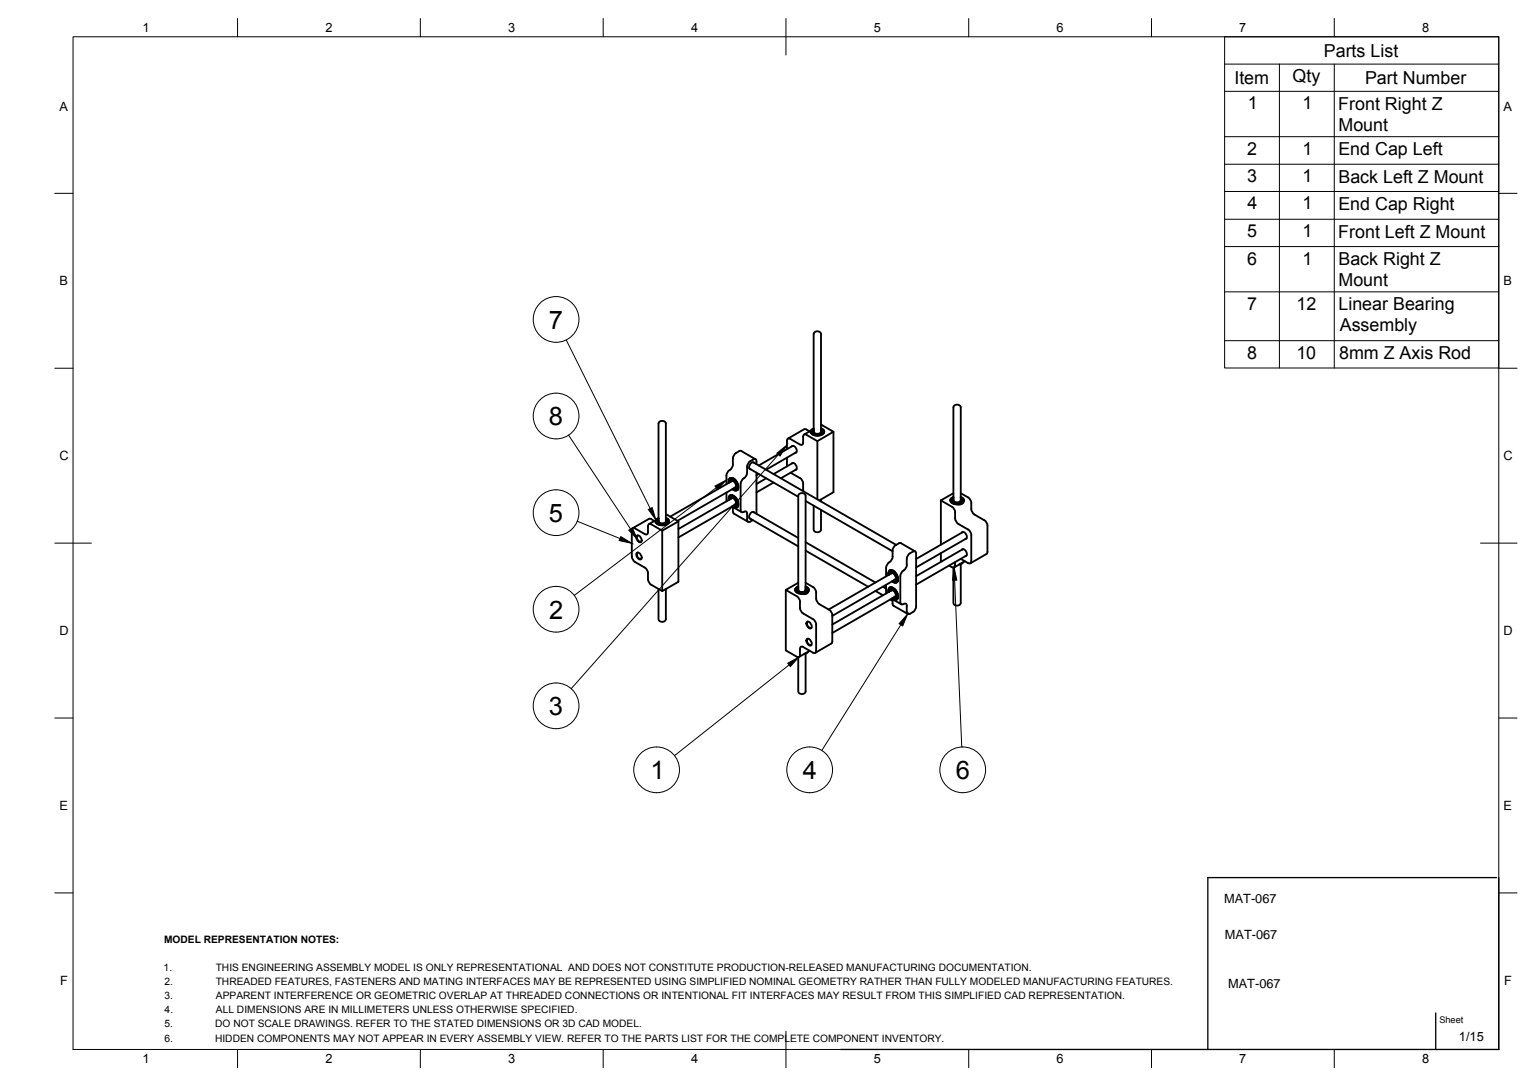
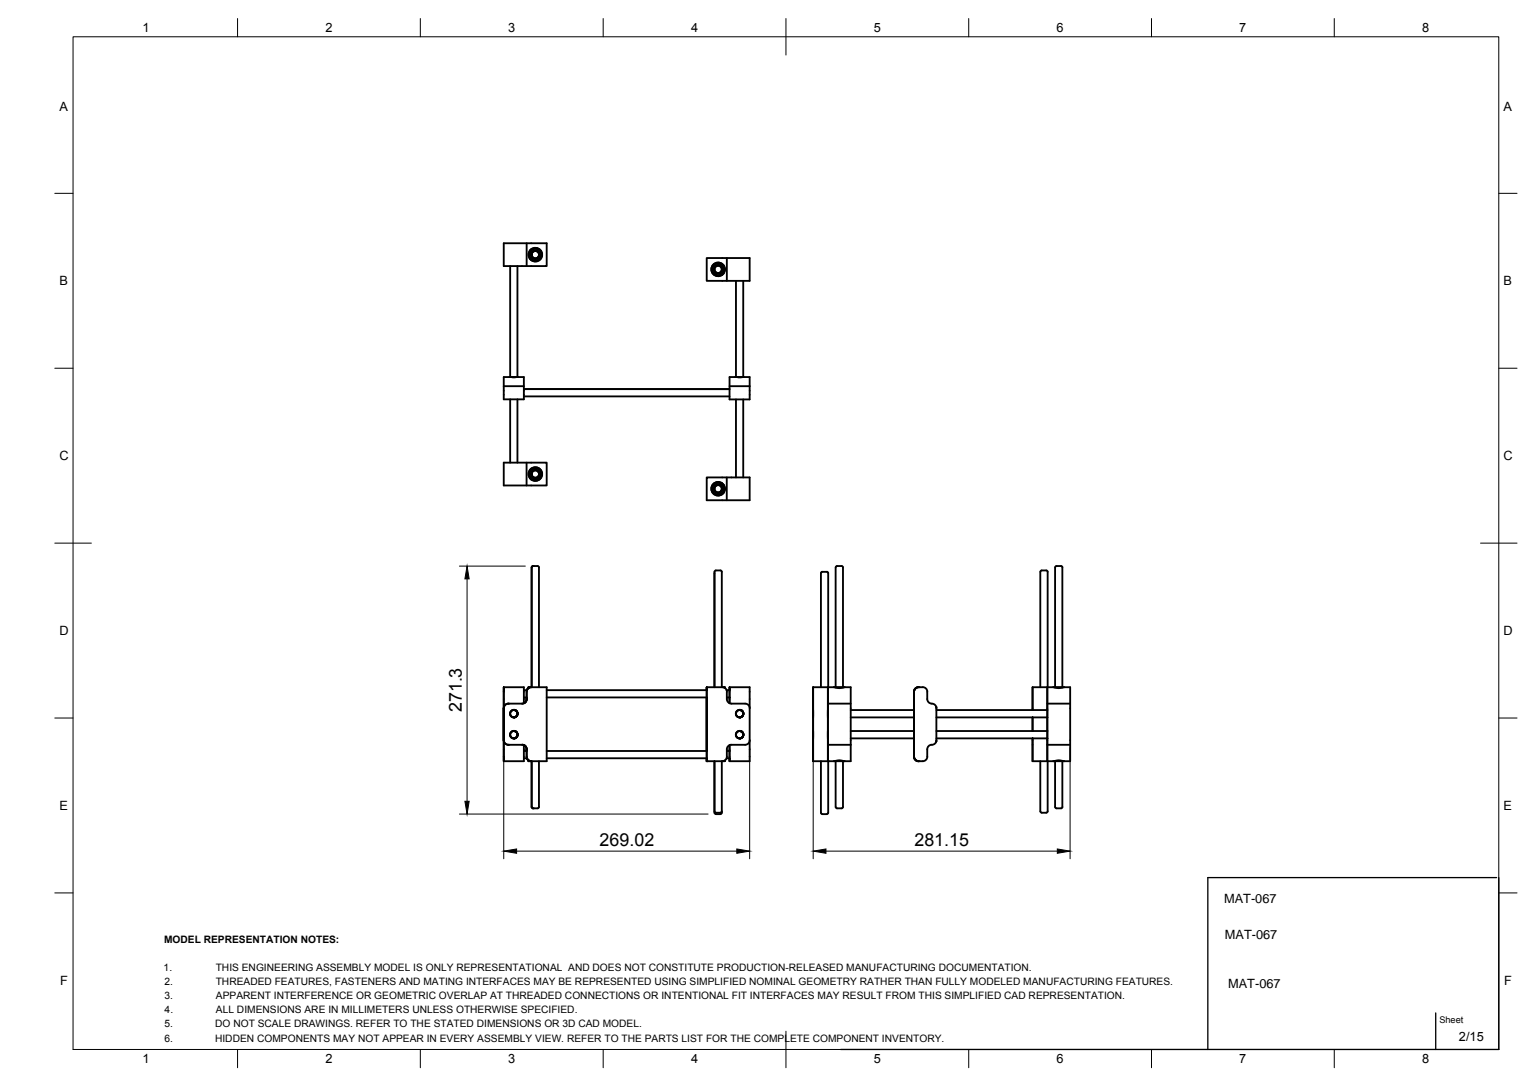
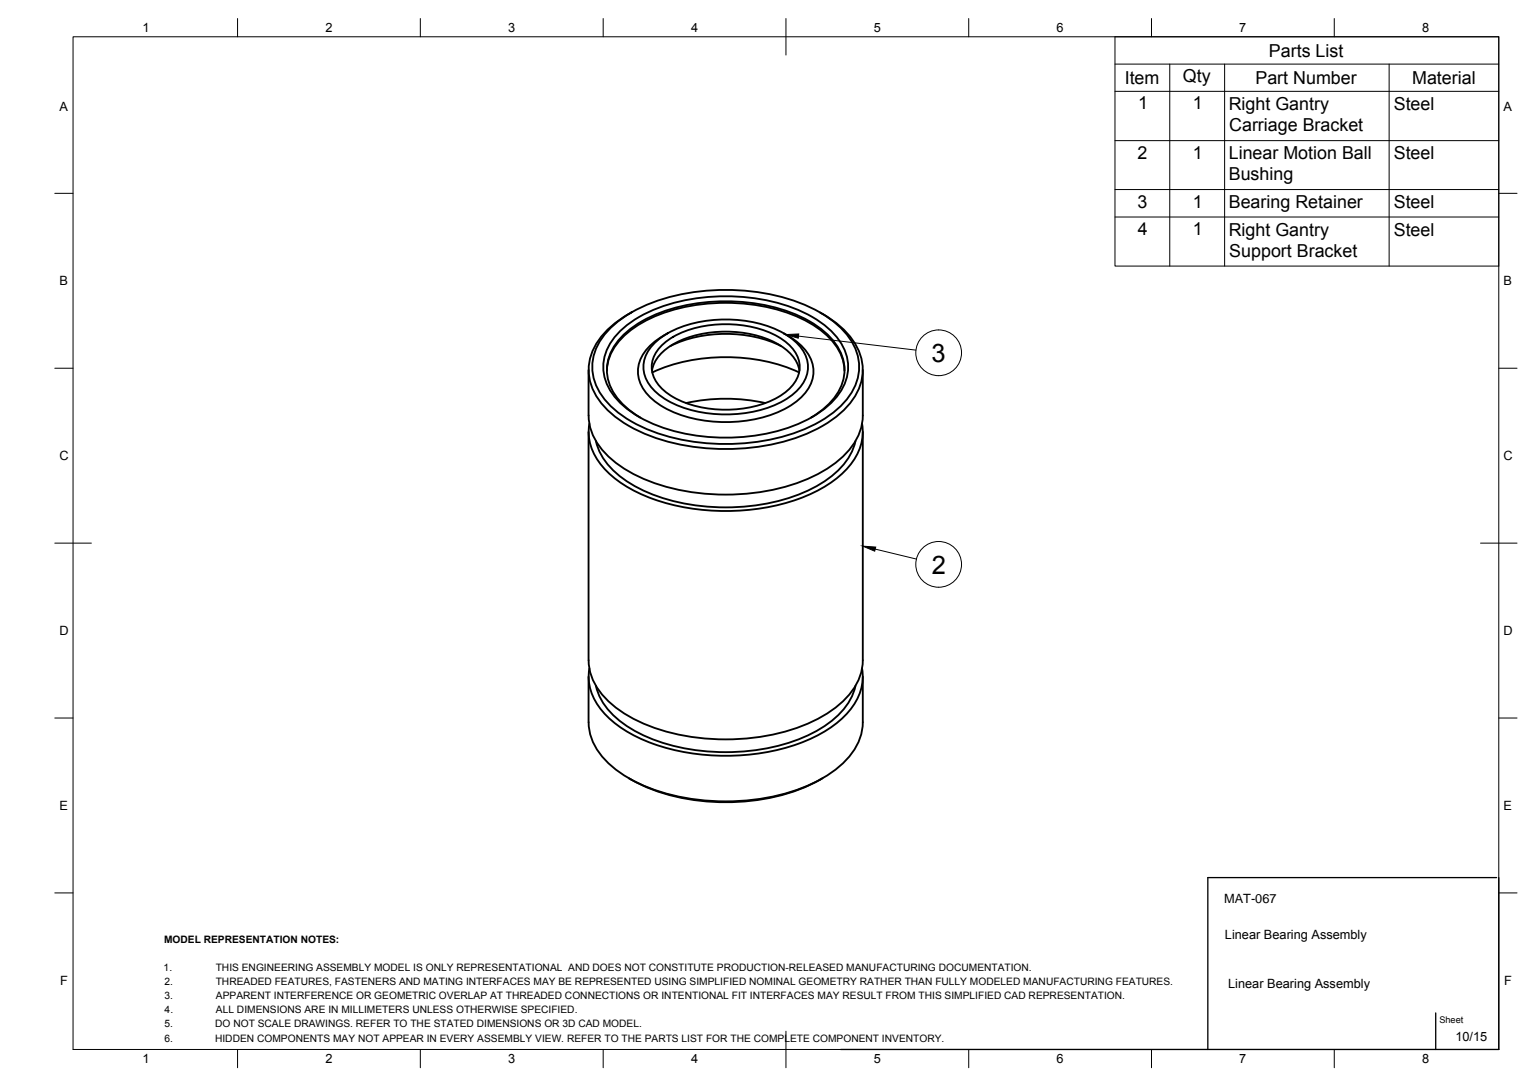
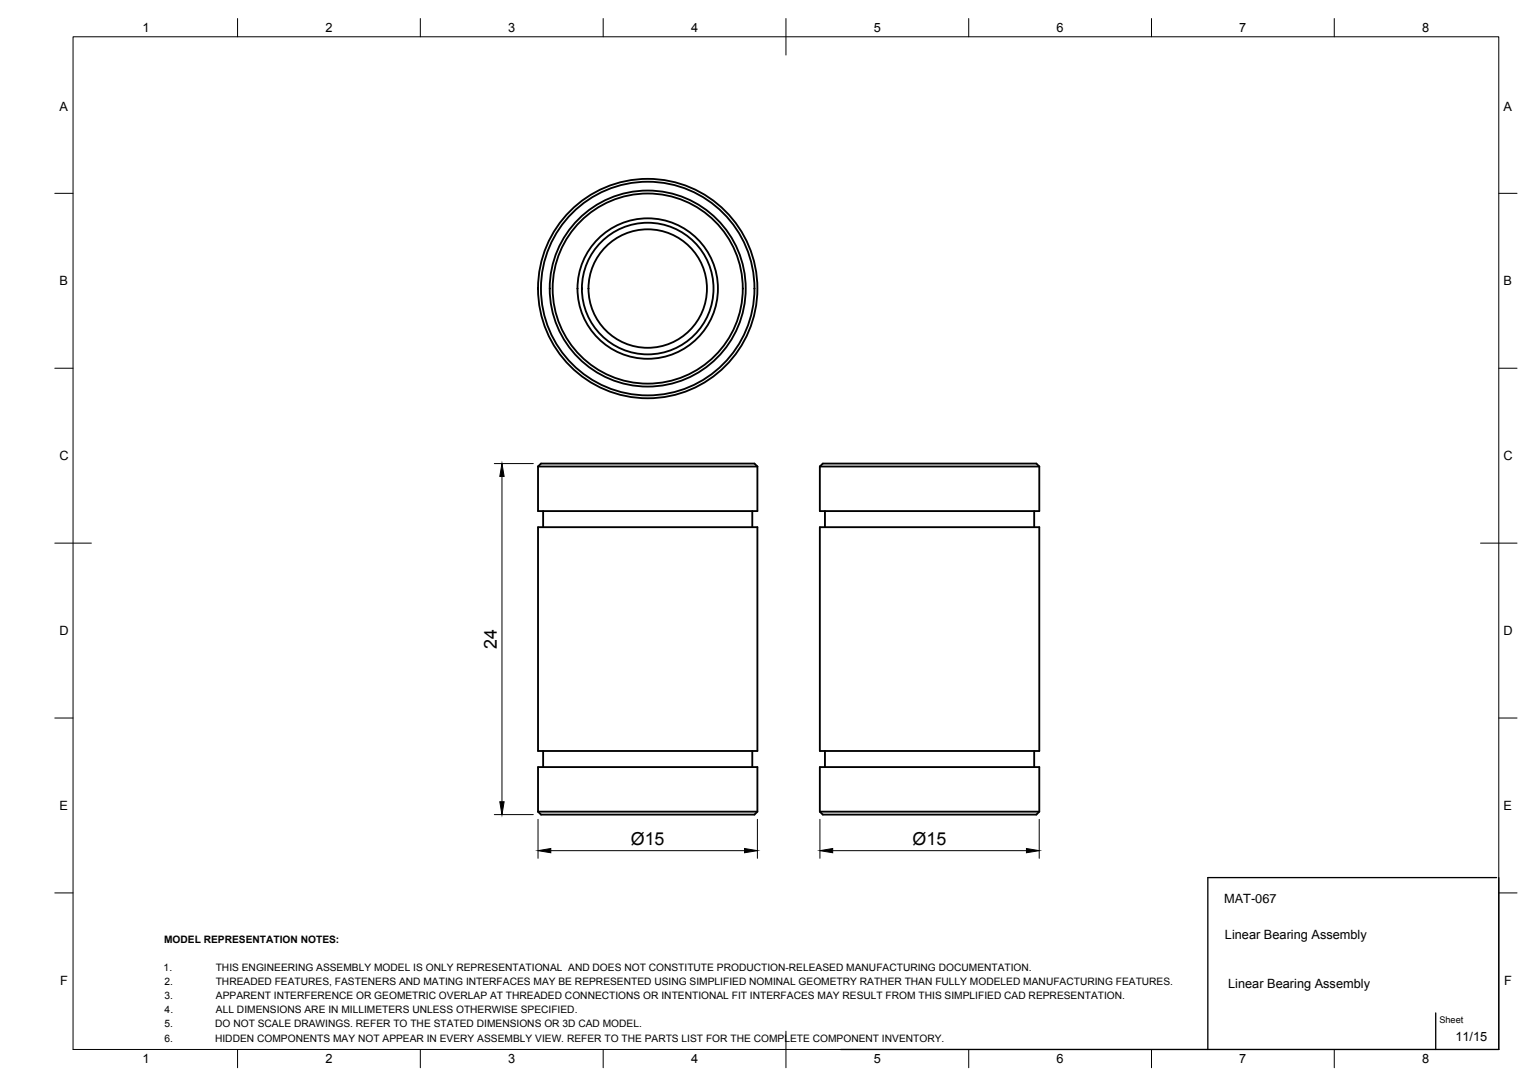
ISO-10303-21;
HEADER;
/* Generated by software containing ST-Developer
 * from STEP Tools, Inc. (www.steptools.com) 
 */

FILE_DESCRIPTION(
/* description */ ('CAx-IF Rec.Pracs.---Representation and Presentation of Product Manufa
cturing Information (PMI)---4.0---2014-10-13'),
/* implementation_level */ '2;1');

FILE_NAME(
/* name */ 'MAT-067',
/* time_stamp */ '2026-10-24T16:02:03-07:00',
/* author */ (''),
/* organization */ (''),
/* preprocessor_version */ 'ST-DEVELOPER v20.2',
/* originating_system */ 'Autodesk Translation Framework v15.17.0.0',
/* authorisation */ '');

FILE_SCHEMA (('AP242_MANAGED_MODEL_BASED_3D_ENGINEERING_MIM_LF { 1 0 10303 442 2 1 4 }'));
ENDSEC;

DATA;
#10=MECHANICAL_DESIGN_GEOMETRIC_PRESENTATION_REPRESENTATION('',(#349,#350,
#351,#352,#353,#354,#355,#356,#357,#358,#359),#6348);
#11=ITEM_DEFINED_TRANSFORMATION($,$,#3804,#3904);
#12=ITEM_DEFINED_TRANSFORMATION($,$,#3865,#3905);
#13=ITEM_DEFINED_TRANSFORMATION($,$,#3880,#3906);
#14=ITEM_DEFINED_TRANSFORMATION($,$,#3895,#3907);
#15=ITEM_DEFINED_TRANSFORMATION($,$,#3804,#3908);
#16=ITEM_DEFINED_TRANSFORMATION($,$,#3865,#3909);
#17=ITEM_DEFINED_TRANSFORMATION($,$,#3880,#3910);
#18=ITEM_DEFINED_TRANSFORMATION($,$,#3895,#3911);
#19=ITEM_DEFINED_TRANSFORMATION($,$,#3804,#3912);
#20=ITEM_DEFINED_TRANSFORMATION($,$,#3865,#3913);
#21=ITEM_DEFINED_TRANSFORMATION($,$,#3880,#3914);
#22=ITEM_DEFINED_TRANSFORMATION($,$,#3895,#3915);
#23=ITEM_DEFINED_TRANSFORMATION($,$,#3804,#3916);
#24=ITEM_DEFINED_TRANSFORMATION($,$,#3865,#3917);
#25=ITEM_DEFINED_TRANSFORMATION($,$,#3880,#3918);
#26=ITEM_DEFINED_TRANSFORMATION($,$,#3895,#3919);
#27=ITEM_DEFINED_TRANSFORMATION($,$,#3804,#3920);
#28=ITEM_DEFINED_TRANSFORMATION($,$,#3865,#3921);
#29=ITEM_DEFINED_TRANSFORMATION($,$,#3880,#3922);
#30=ITEM_DEFINED_TRANSFORMATION($,$,#3895,#3923);
#31=ITEM_DEFINED_TRANSFORMATION($,$,#3804,#3924);
#32=ITEM_DEFINED_TRANSFORMATION($,$,#3865,#3925);
#33=ITEM_DEFINED_TRANSFORMATION($,$,#3880,#3926);
#34=ITEM_DEFINED_TRANSFORMATION($,$,#3895,#3927);
#35=ITEM_DEFINED_TRANSFORMATION($,$,#3804,#3928);
#36=ITEM_DEFINED_TRANSFORMATION($,$,#3865,#3929);
#37=ITEM_DEFINED_TRANSFORMATION($,$,#3880,#3930);
#38=ITEM_DEFINED_TRANSFORMATION($,$,#3895,#3931);
#39=ITEM_DEFINED_TRANSFORMATION($,$,#3804,#3932);
#40=ITEM_DEFINED_TRANSFORMATION($,$,#3865,#3933);
#41=ITEM_DEFINED_TRANSFORMATION($,$,#3880,#3934);
#42=ITEM_DEFINED_TRANSFORMATION($,$,#3895,#3935);
#43=ITEM_DEFINED_TRANSFORMATION($,$,#3804,#3936);
#44=ITEM_DEFINED_TRANSFORMATION($,$,#3865,#3937);
#45=ITEM_DEFINED_TRANSFORMATION($,$,#3880,#3938);
#46=ITEM_DEFINED_TRANSFORMATION($,$,#3895,#3939);
#47=ITEM_DEFINED_TRANSFORMATION($,$,#3804,#3940);
#48=ITEM_DEFINED_TRANSFORMATION($,$,#3865,#3941);
#49=ITEM_DEFINED_TRANSFORMATION($,$,#3880,#3942);
#50=ITEM_DEFINED_TRANSFORMATION($,$,#3895,#3943);
#51=ITEM_DEFINED_TRANSFORMATION($,$,#3804,#3944);
#52=ITEM_DEFINED_TRANSFORMATION($,$,#3865,#3945);
#53=ITEM_DEFINED_TRANSFORMATION($,$,#3880,#3946);
#54=ITEM_DEFINED_TRANSFORMATION($,$,#3895,#3947);
#55=ITEM_DEFINED_TRANSFORMATION($,$,#3804,#3948);
#56=ITEM_DEFINED_TRANSFORMATION($,$,#3865,#3949);
#57=ITEM_DEFINED_TRANSFORMATION($,$,#3880,#3950);
#58=ITEM_DEFINED_TRANSFORMATION($,$,#3895,#3951);
#59=ITEM_DEFINED_TRANSFORMATION($,$,#3522,#3952);
#60=ITEM_DEFINED_TRANSFORMATION($,$,#3562,#3953);
#61=ITEM_DEFINED_TRANSFORMATION($,$,#3602,#3954);
#62=ITEM_DEFINED_TRANSFORMATION($,$,#3642,#3955);
#63=ITEM_DEFINED_TRANSFORMATION($,$,#3682,#3956);
#64=ITEM_DEFINED_TRANSFORMATION($,$,#3779,#3957);
#65=ITEM_DEFINED_TRANSFORMATION($,$,#3779,#3958);
#66=ITEM_DEFINED_TRANSFORMATION($,$,#3779,#3959);
#67=ITEM_DEFINED_TRANSFORMATION($,$,#3779,#3960);
#68=ITEM_DEFINED_TRANSFORMATION($,$,#3779,#3961);
#69=ITEM_DEFINED_TRANSFORMATION($,$,#3779,#3962);
#70=ITEM_DEFINED_TRANSFORMATION($,$,#3779,#3963);
#71=ITEM_DEFINED_TRANSFORMATION($,$,#3683,#3964);
#72=ITEM_DEFINED_TRANSFORMATION($,$,#3731,#3965);
#73=ITEM_DEFINED_TRANSFORMATION($,$,#3779,#3966);
#74=ITEM_DEFINED_TRANSFORMATION($,$,#3779,#3967);
#75=ITEM_DEFINED_TRANSFORMATION($,$,#3779,#3968);
#76=ITEM_DEFINED_TRANSFORMATION($,$,#3793,#3969);
#77=ITEM_DEFINED_TRANSFORMATION($,$,#3794,#3970);
#78=ITEM_DEFINED_TRANSFORMATION($,$,#3795,#3971);
#79=ITEM_DEFINED_TRANSFORMATION($,$,#3796,#3972);
#80=ITEM_DEFINED_TRANSFORMATION($,$,#3797,#3973);
#81=ITEM_DEFINED_TRANSFORMATION($,$,#3798,#3974);
#82=ITEM_DEFINED_TRANSFORMATION($,$,#3799,#3975);
#83=ITEM_DEFINED_TRANSFORMATION($,$,#3800,#3976);
#84=ITEM_DEFINED_TRANSFORMATION($,$,#3801,#3977);
#85=ITEM_DEFINED_TRANSFORMATION($,$,#3802,#3978);
#86=ITEM_DEFINED_TRANSFORMATION($,$,#3803,#3979);
#87=(
REPRESENTATION_RELATIONSHIP($,$,#6496,#6481)
REPRESENTATION_RELATIONSHIP_WITH_TRANSFORMATION(#11)
SHAPE_REPRESENTATION_RELATIONSHIP()
);
#88=(
REPRESENTATION_RELATIONSHIP($,$,#6497,#6481)
REPRESENTATION_RELATIONSHIP_WITH_TRANSFORMATION(#12)
SHAPE_REPRESENTATION_RELATIONSHIP()
);
#89=(
REPRESENTATION_RELATIONSHIP($,$,#6498,#6481)
REPRESENTATION_RELATIONSHIP_WITH_TRANSFORMATION(#13)
SHAPE_REPRESENTATION_RELATIONSHIP()
);
#90=(
REPRESENTATION_RELATIONSHIP($,$,#6499,#6481)
REPRESENTATION_RELATIONSHIP_WITH_TRANSFORMATION(#14)
SHAPE_REPRESENTATION_RELATIONSHIP()
);
#91=(
REPRESENTATION_RELATIONSHIP($,$,#6496,#6485)
REPRESENTATION_RELATIONSHIP_WITH_TRANSFORMATION(#15)
SHAPE_REPRESENTATION_RELATIONSHIP()
);
#92=(
REPRESENTATION_RELATIONSHIP($,$,#6497,#6485)
REPRESENTATION_RELATIONSHIP_WITH_TRANSFORMATION(#16)
SHAPE_REPRESENTATION_RELATIONSHIP()
);
#93=(
REPRESENTATION_RELATIONSHIP($,$,#6498,#6485)
REPRESENTATION_RELATIONSHIP_WITH_TRANSFORMATION(#17)
SHAPE_REPRESENTATION_RELATIONSHIP()
);
#94=(
REPRESENTATION_RELATIONSHIP($,$,#6499,#6485)
REPRESENTATION_RELATIONSHIP_WITH_TRANSFORMATION(#18)
SHAPE_REPRESENTATION_RELATIONSHIP()
);
#95=(
REPRESENTATION_RELATIONSHIP($,$,#6496,#6486)
REPRESENTATION_RELATIONSHIP_WITH_TRANSFORMATION(#19)
SHAPE_REPRESENTATION_RELATIONSHIP()
);
#96=(
REPRESENTATION_RELATIONSHIP($,$,#6497,#6486)
REPRESENTATION_RELATIONSHIP_WITH_TRANSFORMATION(#20)
SHAPE_REPRESENTATION_RELATIONSHIP()
);
#97=(
REPRESENTATION_RELATIONSHIP($,$,#6498,#6486)
REPRESENTATION_RELATIONSHIP_WITH_TRANSFORMATION(#21)
SHAPE_REPRESENTATION_RELATIONSHIP()
);
#98=(
REPRESENTATION_RELATIONSHIP($,$,#6499,#6486)
REPRESENTATION_RELATIONSHIP_WITH_TRANSFORMATION(#22)
SHAPE_REPRESENTATION_RELATIONSHIP()
);
#99=(
REPRESENTATION_RELATIONSHIP($,$,#6496,#6487)
REPRESENTATION_RELATIONSHIP_WITH_TRANSFORMATION(#23)
SHAPE_REPRESENTATION_RELATIONSHIP()
);
#100=(
REPRESENTATION_RELATIONSHIP($,$,#6497,#6487)
REPRESENTATION_RELATIONSHIP_WITH_TRANSFORMATION(#24)
SHAPE_REPRESENTATION_RELATIONSHIP()
);
#101=(
REPRESENTATION_RELATIONSHIP($,$,#6498,#6487)
REPRESENTATION_RELATIONSHIP_WITH_TRANSFORMATION(#25)
SHAPE_REPRESENTATION_RELATIONSHIP()
);
#102=(
REPRESENTATION_RELATIONSHIP($,$,#6499,#6487)
REPRESENTATION_RELATIONSHIP_WITH_TRANSFORMATION(#26)
SHAPE_REPRESENTATION_RELATIONSHIP()
);
#103=(
REPRESENTATION_RELATIONSHIP($,$,#6496,#6488)
REPRESENTATION_RELATIONSHIP_WITH_TRANSFORMATION(#27)
SHAPE_REPRESENTATION_RELATIONSHIP()
);
#104=(
REPRESENTATION_RELATIONSHIP($,$,#6497,#6488)
REPRESENTATION_RELATIONSHIP_WITH_TRANSFORMATION(#28)
SHAPE_REPRESENTATION_RELATIONSHIP()
);
#105=(
REPRESENTATION_RELATIONSHIP($,$,#6498,#6488)
REPRESENTATION_RELATIONSHIP_WITH_TRANSFORMATION(#29)
SHAPE_REPRESENTATION_RELATIONSHIP()
);
#106=(
REPRESENTATION_RELATIONSHIP($,$,#6499,#6488)
REPRESENTATION_RELATIONSHIP_WITH_TRANSFORMATION(#30)
SHAPE_REPRESENTATION_RELATIONSHIP()
);
#107=(
REPRESENTATION_RELATIONSHIP($,$,#6496,#6489)
REPRESENTATION_RELATIONSHIP_WITH_TRANSFORMATION(#31)
SHAPE_REPRESENTATION_RELATIONSHIP()
);
#108=(
REPRESENTATION_RELATIONSHIP($,$,#6497,#6489)
REPRESENTATION_RELATIONSHIP_WITH_TRANSFORMATION(#32)
SHAPE_REPRESENTATION_RELATIONSHIP()
);
#109=(
REPRESENTATION_RELATIONSHIP($,$,#6498,#6489)
REPRESENTATION_RELATIONSHIP_WITH_TRANSFORMATION(#33)
SHAPE_REPRESENTATION_RELATIONSHIP()
);
#110=(
REPRESENTATION_RELATIONSHIP($,$,#6499,#6489)
REPRESENTATION_RELATIONSHIP_WITH_TRANSFORMATION(#34)
SHAPE_REPRESENTATION_RELATIONSHIP()
);
#111=(
REPRESENTATION_RELATIONSHIP($,$,#6496,#6490)
REPRESENTATION_RELATIONSHIP_WITH_TRANSFORMATION(#35)
SHAPE_REPRESENTATION_RELATIONSHIP()
);
#112=(
REPRESENTATION_RELATIONSHIP($,$,#6497,#6490)
REPRESENTATION_RELATIONSHIP_WITH_TRANSFORMATION(#36)
SHAPE_REPRESENTATION_RELATIONSHIP()
);
#113=(
REPRESENTATION_RELATIONSHIP($,$,#6498,#6490)
REPRESENTATION_RELATIONSHIP_WITH_TRANSFORMATION(#37)
SHAPE_REPRESENTATION_RELATIONSHIP()
);
#114=(
REPRESENTATION_RELATIONSHIP($,$,#6499,#6490)
REPRESENTATION_RELATIONSHIP_WITH_TRANSFORMATION(#38)
SHAPE_REPRESENTATION_RELATIONSHIP()
);
#115=(
REPRESENTATION_RELATIONSHIP($,$,#6496,#6491)
REPRESENTATION_RELATIONSHIP_WITH_TRANSFORMATION(#39)
SHAPE_REPRESENTATION_RELATIONSHIP()
);
#116=(
REPRESENTATION_RELATIONSHIP($,$,#6497,#6491)
REPRESENTATION_RELATIONSHIP_WITH_TRANSFORMATION(#40)
SHAPE_REPRESENTATION_RELATIONSHIP()
);
#117=(
REPRESENTATION_RELATIONSHIP($,$,#6498,#6491)
REPRESENTATION_RELATIONSHIP_WITH_TRANSFORMATION(#41)
SHAPE_REPRESENTATION_RELATIONSHIP()
);
#118=(
REPRESENTATION_RELATIONSHIP($,$,#6499,#6491)
REPRESENTATION_RELATIONSHIP_WITH_TRANSFORMATION(#42)
SHAPE_REPRESENTATION_RELATIONSHIP()
);
#119=(
REPRESENTATION_RELATIONSHIP($,$,#6496,#6492)
REPRESENTATION_RELATIONSHIP_WITH_TRANSFORMATION(#43)
SHAPE_REPRESENTATION_RELATIONSHIP()
);
#120=(
REPRESENTATION_RELATIONSHIP($,$,#6497,#6492)
REPRESENTATION_RELATIONSHIP_WITH_TRANSFORMATION(#44)
SHAPE_REPRESENTATION_RELATIONSHIP()
);
#121=(
REPRESENTATION_RELATIONSHIP($,$,#6498,#6492)
REPRESENTATION_RELATIONSHIP_WITH_TRANSFORMATION(#45)
SHAPE_REPRESENTATION_RELATIONSHIP()
);
#122=(
REPRESENTATION_RELATIONSHIP($,$,#6499,#6492)
REPRESENTATION_RELATIONSHIP_WITH_TRANSFORMATION(#46)
SHAPE_REPRESENTATION_RELATIONSHIP()
);
#123=(
REPRESENTATION_RELATIONSHIP($,$,#6496,#6493)
REPRESENTATION_RELATIONSHIP_WITH_TRANSFORMATION(#47)
SHAPE_REPRESENTATION_RELATIONSHIP()
);
#124=(
REPRESENTATION_RELATIONSHIP($,$,#6497,#6493)
REPRESENTATION_RELATIONSHIP_WITH_TRANSFORMATION(#48)
SHAPE_REPRESENTATION_RELATIONSHIP()
);
#125=(
REPRESENTATION_RELATIONSHIP($,$,#6498,#6493)
REPRESENTATION_RELATIONSHIP_WITH_TRANSFORMATION(#49)
SHAPE_REPRESENTATION_RELATIONSHIP()
);
#126=(
REPRESENTATION_RELATIONSHIP($,$,#6499,#6493)
REPRESENTATION_RELATIONSHIP_WITH_TRANSFORMATION(#50)
SHAPE_REPRESENTATION_RELATIONSHIP()
);
#127=(
REPRESENTATION_RELATIONSHIP($,$,#6496,#6494)
REPRESENTATION_RELATIONSHIP_WITH_TRANSFORMATION(#51)
SHAPE_REPRESENTATION_RELATIONSHIP()
);
#128=(
REPRESENTATION_RELATIONSHIP($,$,#6497,#6494)
REPRESENTATION_RELATIONSHIP_WITH_TRANSFORMATION(#52)
SHAPE_REPRESENTATION_RELATIONSHIP()
);
#129=(
REPRESENTATION_RELATIONSHIP($,$,#6498,#6494)
REPRESENTATION_RELATIONSHIP_WITH_TRANSFORMATION(#53)
SHAPE_REPRESENTATION_RELATIONSHIP()
);
#130=(
REPRESENTATION_RELATIONSHIP($,$,#6499,#6494)
REPRESENTATION_RELATIONSHIP_WITH_TRANSFORMATION(#54)
SHAPE_REPRESENTATION_RELATIONSHIP()
);
#131=(
REPRESENTATION_RELATIONSHIP($,$,#6496,#6495)
REPRESENTATION_RELATIONSHIP_WITH_TRANSFORMATION(#55)
SHAPE_REPRESENTATION_RELATIONSHIP()
);
#132=(
REPRESENTATION_RELATIONSHIP($,$,#6497,#6495)
REPRESENTATION_RELATIONSHIP_WITH_TRANSFORMATION(#56)
SHAPE_REPRESENTATION_RELATIONSHIP()
);
#133=(
REPRESENTATION_RELATIONSHIP($,$,#6498,#6495)
REPRESENTATION_RELATIONSHIP_WITH_TRANSFORMATION(#57)
SHAPE_REPRESENTATION_RELATIONSHIP()
);
#134=(
REPRESENTATION_RELATIONSHIP($,$,#6499,#6495)
REPRESENTATION_RELATIONSHIP_WITH_TRANSFORMATION(#58)
SHAPE_REPRESENTATION_RELATIONSHIP()
);
#135=(
REPRESENTATION_RELATIONSHIP($,$,#6477,#6476)
REPRESENTATION_RELATIONSHIP_WITH_TRANSFORMATION(#59)
SHAPE_REPRESENTATION_RELATIONSHIP()
);
#136=(
REPRESENTATION_RELATIONSHIP($,$,#6478,#6476)
REPRESENTATION_RELATIONSHIP_WITH_TRANSFORMATION(#60)
SHAPE_REPRESENTATION_RELATIONSHIP()
);
#137=(
REPRESENTATION_RELATIONSHIP($,$,#6479,#6476)
REPRESENTATION_RELATIONSHIP_WITH_TRANSFORMATION(#61)
SHAPE_REPRESENTATION_RELATIONSHIP()
);
#138=(
REPRESENTATION_RELATIONSHIP($,$,#6480,#6476)
REPRESENTATION_RELATIONSHIP_WITH_TRANSFORMATION(#62)
SHAPE_REPRESENTATION_RELATIONSHIP()
);
#139=(
REPRESENTATION_RELATIONSHIP($,$,#6481,#6476)
REPRESENTATION_RELATIONSHIP_WITH_TRANSFORMATION(#63)
SHAPE_REPRESENTATION_RELATIONSHIP()
);
#140=(
REPRESENTATION_RELATIONSHIP($,$,#6484,#6476)
REPRESENTATION_RELATIONSHIP_WITH_TRANSFORMATION(#64)
SHAPE_REPRESENTATION_RELATIONSHIP()
);
#141=(
REPRESENTATION_RELATIONSHIP($,$,#6484,#6476)
REPRESENTATION_RELATIONSHIP_WITH_TRANSFORMATION(#65)
SHAPE_REPRESENTATION_RELATIONSHIP()
);
#142=(
REPRESENTATION_RELATIONSHIP($,$,#6484,#6476)
REPRESENTATION_RELATIONSHIP_WITH_TRANSFORMATION(#66)
SHAPE_REPRESENTATION_RELATIONSHIP()
);
#143=(
REPRESENTATION_RELATIONSHIP($,$,#6484,#6476)
REPRESENTATION_RELATIONSHIP_WITH_TRANSFORMATION(#67)
SHAPE_REPRESENTATION_RELATIONSHIP()
);
#144=(
REPRESENTATION_RELATIONSHIP($,$,#6484,#6476)
REPRESENTATION_RELATIONSHIP_WITH_TRANSFORMATION(#68)
SHAPE_REPRESENTATION_RELATIONSHIP()
);
#145=(
REPRESENTATION_RELATIONSHIP($,$,#6484,#6476)
REPRESENTATION_RELATIONSHIP_WITH_TRANSFORMATION(#69)
SHAPE_REPRESENTATION_RELATIONSHIP()
);
#146=(
REPRESENTATION_RELATIONSHIP($,$,#6484,#6476)
REPRESENTATION_RELATIONSHIP_WITH_TRANSFORMATION(#70)
SHAPE_REPRESENTATION_RELATIONSHIP()
);
#147=(
REPRESENTATION_RELATIONSHIP($,$,#6482,#6476)
REPRESENTATION_RELATIONSHIP_WITH_TRANSFORMATION(#71)
SHAPE_REPRESENTATION_RELATIONSHIP()
);
#148=(
REPRESENTATION_RELATIONSHIP($,$,#6483,#6476)
REPRESENTATION_RELATIONSHIP_WITH_TRANSFORMATION(#72)
SHAPE_REPRESENTATION_RELATIONSHIP()
);
#149=(
REPRESENTATION_RELATIONSHIP($,$,#6484,#6476)
REPRESENTATION_RELATIONSHIP_WITH_TRANSFORMATION(#73)
SHAPE_REPRESENTATION_RELATIONSHIP()
);
#150=(
REPRESENTATION_RELATIONSHIP($,$,#6484,#6476)
REPRESENTATION_RELATIONSHIP_WITH_TRANSFORMATION(#74)
SHAPE_REPRESENTATION_RELATIONSHIP()
);
#151=(
REPRESENTATION_RELATIONSHIP($,$,#6484,#6476)
REPRESENTATION_RELATIONSHIP_WITH_TRANSFORMATION(#75)
SHAPE_REPRESENTATION_RELATIONSHIP()
);
#152=(
REPRESENTATION_RELATIONSHIP($,$,#6485,#6476)
REPRESENTATION_RELATIONSHIP_WITH_TRANSFORMATION(#76)
SHAPE_REPRESENTATION_RELATIONSHIP()
);
#153=(
REPRESENTATION_RELATIONSHIP($,$,#6486,#6476)
REPRESENTATION_RELATIONSHIP_WITH_TRANSFORMATION(#77)
SHAPE_REPRESENTATION_RELATIONSHIP()
);
#154=(
REPRESENTATION_RELATIONSHIP($,$,#6487,#6476)
REPRESENTATION_RELATIONSHIP_WITH_TRANSFORMATION(#78)
SHAPE_REPRESENTATION_RELATIONSHIP()
);
#155=(
REPRESENTATION_RELATIONSHIP($,$,#6488,#6476)
REPRESENTATION_RELATIONSHIP_WITH_TRANSFORMATION(#79)
SHAPE_REPRESENTATION_RELATIONSHIP()
);
#156=(
REPRESENTATION_RELATIONSHIP($,$,#6489,#6476)
REPRESENTATION_RELATIONSHIP_WITH_TRANSFORMATION(#80)
SHAPE_REPRESENTATION_RELATIONSHIP()
);
#157=(
REPRESENTATION_RELATIONSHIP($,$,#6490,#6476)
REPRESENTATION_RELATIONSHIP_WITH_TRANSFORMATION(#81)
SHAPE_REPRESENTATION_RELATIONSHIP()
);
#158=(
REPRESENTATION_RELATIONSHIP($,$,#6491,#6476)
REPRESENTATION_RELATIONSHIP_WITH_TRANSFORMATION(#82)
SHAPE_REPRESENTATION_RELATIONSHIP()
);
#159=(
REPRESENTATION_RELATIONSHIP($,$,#6492,#6476)
REPRESENTATION_RELATIONSHIP_WITH_TRANSFORMATION(#83)
SHAPE_REPRESENTATION_RELATIONSHIP()
);
#160=(
REPRESENTATION_RELATIONSHIP($,$,#6493,#6476)
REPRESENTATION_RELATIONSHIP_WITH_TRANSFORMATION(#84)
SHAPE_REPRESENTATION_RELATIONSHIP()
);
#161=(
REPRESENTATION_RELATIONSHIP($,$,#6494,#6476)
REPRESENTATION_RELATIONSHIP_WITH_TRANSFORMATION(#85)
SHAPE_REPRESENTATION_RELATIONSHIP()
);
#162=(
REPRESENTATION_RELATIONSHIP($,$,#6495,#6476)
REPRESENTATION_RELATIONSHIP_WITH_TRANSFORMATION(#86)
SHAPE_REPRESENTATION_RELATIONSHIP()
);
#163=CONTEXT_DEPENDENT_SHAPE_REPRESENTATION(#87,#6400);
#164=CONTEXT_DEPENDENT_SHAPE_REPRESENTATION(#88,#6401);
#165=CONTEXT_DEPENDENT_SHAPE_REPRESENTATION(#89,#6402);
#166=CONTEXT_DEPENDENT_SHAPE_REPRESENTATION(#90,#6403);
#167=CONTEXT_DEPENDENT_SHAPE_REPRESENTATION(#91,#6404);
#168=CONTEXT_DEPENDENT_SHAPE_REPRESENTATION(#92,#6405);
#169=CONTEXT_DEPENDENT_SHAPE_REPRESENTATION(#93,#6406);
#170=CONTEXT_DEPENDENT_SHAPE_REPRESENTATION(#94,#6407);
#171=CONTEXT_DEPENDENT_SHAPE_REPRESENTATION(#95,#6408);
#172=CONTEXT_DEPENDENT_SHAPE_REPRESENTATION(#96,#6409);
#173=CONTEXT_DEPENDENT_SHAPE_REPRESENTATION(#97,#6410);
#174=CONTEXT_DEPENDENT_SHAPE_REPRESENTATION(#98,#6411);
#175=CONTEXT_DEPENDENT_SHAPE_REPRESENTATION(#99,#6412);
#176=CONTEXT_DEPENDENT_SHAPE_REPRESENTATION(#100,#6413);
#177=CONTEXT_DEPENDENT_SHAPE_REPRESENTATION(#101,#6414);
#178=CONTEXT_DEPENDENT_SHAPE_REPRESENTATION(#102,#6415);
#179=CONTEXT_DEPENDENT_SHAPE_REPRESENTATION(#103,#6416);
#180=CONTEXT_DEPENDENT_SHAPE_REPRESENTATION(#104,#6417);
#181=CONTEXT_DEPENDENT_SHAPE_REPRESENTATION(#105,#6418);
#182=CONTEXT_DEPENDENT_SHAPE_REPRESENTATION(#106,#6419);
#183=CONTEXT_DEPENDENT_SHAPE_REPRESENTATION(#107,#6420);
#184=CONTEXT_DEPENDENT_SHAPE_REPRESENTATION(#108,#6421);
#185=CONTEXT_DEPENDENT_SHAPE_REPRESENTATION(#109,#6422);
#186=CONTEXT_DEPENDENT_SHAPE_REPRESENTATION(#110,#6423);
#187=CONTEXT_DEPENDENT_SHAPE_REPRESENTATION(#111,#6424);
#188=CONTEXT_DEPENDENT_SHAPE_REPRESENTATION(#112,#6425);
#189=CONTEXT_DEPENDENT_SHAPE_REPRESENTATION(#113,#6426);
#190=CONTEXT_DEPENDENT_SHAPE_REPRESENTATION(#114,#6427);
#191=CONTEXT_DEPENDENT_SHAPE_REPRESENTATION(#115,#6428);
#192=CONTEXT_DEPENDENT_SHAPE_REPRESENTATION(#116,#6429);
#193=CONTEXT_DEPENDENT_SHAPE_REPRESENTATION(#117,#6430);
#194=CONTEXT_DEPENDENT_SHAPE_REPRESENTATION(#118,#6431);
#195=CONTEXT_DEPENDENT_SHAPE_REPRESENTATION(#119,#6432);
#196=CONTEXT_DEPENDENT_SHAPE_REPRESENTATION(#120,#6433);
#197=CONTEXT_DEPENDENT_SHAPE_REPRESENTATION(#121,#6434);
#198=CONTEXT_DEPENDENT_SHAPE_REPRESENTATION(#122,#6435);
#199=CONTEXT_DEPENDENT_SHAPE_REPRESENTATION(#123,#6436);
#200=CONTEXT_DEPENDENT_SHAPE_REPRESENTATION(#124,#6437);
#201=CONTEXT_DEPENDENT_SHAPE_REPRESENTATION(#125,#6438);
#202=CONTEXT_DEPENDENT_SHAPE_REPRESENTATION(#126,#6439);
#203=CONTEXT_DEPENDENT_SHAPE_REPRESENTATION(#127,#6440);
#204=CONTEXT_DEPENDENT_SHAPE_REPRESENTATION(#128,#6441);
#205=CONTEXT_DEPENDENT_SHAPE_REPRESENTATION(#129,#6442);
#206=CONTEXT_DEPENDENT_SHAPE_REPRESENTATION(#130,#6443);
#207=CONTEXT_DEPENDENT_SHAPE_REPRESENTATION(#131,#6444);
#208=CONTEXT_DEPENDENT_SHAPE_REPRESENTATION(#132,#6445);
#209=CONTEXT_DEPENDENT_SHAPE_REPRESENTATION(#133,#6446);
#210=CONTEXT_DEPENDENT_SHAPE_REPRESENTATION(#134,#6447);
#211=CONTEXT_DEPENDENT_SHAPE_REPRESENTATION(#135,#6448);
#212=CONTEXT_DEPENDENT_SHAPE_REPRESENTATION(#136,#6449);
#213=CONTEXT_DEPENDENT_SHAPE_REPRESENTATION(#137,#6450);
#214=CONTEXT_DEPENDENT_SHAPE_REPRESENTATION(#138,#6451);
#215=CONTEXT_DEPENDENT_SHAPE_REPRESENTATION(#139,#6452);
#216=CONTEXT_DEPENDENT_SHAPE_REPRESENTATION(#140,#6453);
#217=CONTEXT_DEPENDENT_SHAPE_REPRESENTATION(#141,#6454);
#218=CONTEXT_DEPENDENT_SHAPE_REPRESENTATION(#142,#6455);
#219=CONTEXT_DEPENDENT_SHAPE_REPRESENTATION(#143,#6456);
#220=CONTEXT_DEPENDENT_SHAPE_REPRESENTATION(#144,#6457);
#221=CONTEXT_DEPENDENT_SHAPE_REPRESENTATION(#145,#6458);
#222=CONTEXT_DEPENDENT_SHAPE_REPRESENTATION(#146,#6459);
#223=CONTEXT_DEPENDENT_SHAPE_REPRESENTATION(#147,#6460);
#224=CONTEXT_DEPENDENT_SHAPE_REPRESENTATION(#148,#6461);
#225=CONTEXT_DEPENDENT_SHAPE_REPRESENTATION(#149,#6462);
#226=CONTEXT_DEPENDENT_SHAPE_REPRESENTATION(#150,#6463);
#227=CONTEXT_DEPENDENT_SHAPE_REPRESENTATION(#151,#6464);
#228=CONTEXT_DEPENDENT_SHAPE_REPRESENTATION(#152,#6465);
#229=CONTEXT_DEPENDENT_SHAPE_REPRESENTATION(#153,#6466);
#230=CONTEXT_DEPENDENT_SHAPE_REPRESENTATION(#154,#6467);
#231=CONTEXT_DEPENDENT_SHAPE_REPRESENTATION(#155,#6468);
#232=CONTEXT_DEPENDENT_SHAPE_REPRESENTATION(#156,#6469);
#233=CONTEXT_DEPENDENT_SHAPE_REPRESENTATION(#157,#6470);
#234=CONTEXT_DEPENDENT_SHAPE_REPRESENTATION(#158,#6471);
#235=CONTEXT_DEPENDENT_SHAPE_REPRESENTATION(#159,#6472);
#236=CONTEXT_DEPENDENT_SHAPE_REPRESENTATION(#160,#6473);
#237=CONTEXT_DEPENDENT_SHAPE_REPRESENTATION(#161,#6474);
#238=CONTEXT_DEPENDENT_SHAPE_REPRESENTATION(#162,#6475);
#239=NEXT_ASSEMBLY_USAGE_OCCURRENCE('Linear Motion Ball Bushing:1',
'Linear Motion Ball Bushing:1','Linear Motion Ball Bushing:1',#6506,#6521,
'Linear Motion Ball Bushing:1');
#240=NEXT_ASSEMBLY_USAGE_OCCURRENCE('Right Gantry Carriage Bracket:1',
'Right Gantry Carriage Bracket:1','Right Gantry Carriage Bracket:1',#6506,
#6522,'Right Gantry Carriage Bracket:1');
#241=NEXT_ASSEMBLY_USAGE_OCCURRENCE('Bearing Retainer:1',
'Bearing Retainer:1','Bearing Retainer:1',#6506,#6523,
'Bearing Retainer:1');
#242=NEXT_ASSEMBLY_USAGE_OCCURRENCE('Right Gantry Support Bracket:1',
'Right Gantry Support Bracket:1','Right Gantry Support Bracket:1',#6506,
#6524,'Right Gantry Support Bracket:1');
#243=NEXT_ASSEMBLY_USAGE_OCCURRENCE('Linear Motion Ball Bushing:1',
'Linear Motion Ball Bushing:1','Linear Motion Ball Bushing:1',#6510,#6521,
'Linear Motion Ball Bushing:1');
#244=NEXT_ASSEMBLY_USAGE_OCCURRENCE('Right Gantry Carriage Bracket:1',
'Right Gantry Carriage Bracket:1','Right Gantry Carriage Bracket:1',#6510,
#6522,'Right Gantry Carriage Bracket:1');
#245=NEXT_ASSEMBLY_USAGE_OCCURRENCE('Bearing Retainer:1',
'Bearing Retainer:1','Bearing Retainer:1',#6510,#6523,
'Bearing Retainer:1');
#246=NEXT_ASSEMBLY_USAGE_OCCURRENCE('Right Gantry Support Bracket:1',
'Right Gantry Support Bracket:1','Right Gantry Support Bracket:1',#6510,
#6524,'Right Gantry Support Bracket:1');
#247=NEXT_ASSEMBLY_USAGE_OCCURRENCE('Linear Motion Ball Bushing:1',
'Linear Motion Ball Bushing:1','Linear Motion Ball Bushing:1',#6511,#6521,
'Linear Motion Ball Bushing:1');
#248=NEXT_ASSEMBLY_USAGE_OCCURRENCE('Right Gantry Carriage Bracket:1',
'Right Gantry Carriage Bracket:1','Right Gantry Carriage Bracket:1',#6511,
#6522,'Right Gantry Carriage Bracket:1');
#249=NEXT_ASSEMBLY_USAGE_OCCURRENCE('Bearing Retainer:1',
'Bearing Retainer:1','Bearing Retainer:1',#6511,#6523,
'Bearing Retainer:1');
#250=NEXT_ASSEMBLY_USAGE_OCCURRENCE('Right Gantry Support Bracket:1',
'Right Gantry Support Bracket:1','Right Gantry Support Bracket:1',#6511,
#6524,'Right Gantry Support Bracket:1');
#251=NEXT_ASSEMBLY_USAGE_OCCURRENCE('Linear Motion Ball Bushing:1',
'Linear Motion Ball Bushing:1','Linear Motion Ball Bushing:1',#6512,#6521,
'Linear Motion Ball Bushing:1');
#252=NEXT_ASSEMBLY_USAGE_OCCURRENCE('Right Gantry Carriage Bracket:1',
'Right Gantry Carriage Bracket:1','Right Gantry Carriage Bracket:1',#6512,
#6522,'Right Gantry Carriage Bracket:1');
#253=NEXT_ASSEMBLY_USAGE_OCCURRENCE('Bearing Retainer:1',
'Bearing Retainer:1','Bearing Retainer:1',#6512,#6523,
'Bearing Retainer:1');
#254=NEXT_ASSEMBLY_USAGE_OCCURRENCE('Right Gantry Support Bracket:1',
'Right Gantry Support Bracket:1','Right Gantry Support Bracket:1',#6512,
#6524,'Right Gantry Support Bracket:1');
#255=NEXT_ASSEMBLY_USAGE_OCCURRENCE('Linear Motion Ball Bushing:1',
'Linear Motion Ball Bushing:1','Linear Motion Ball Bushing:1',#6513,#6521,
'Linear Motion Ball Bushing:1');
#256=NEXT_ASSEMBLY_USAGE_OCCURRENCE('Right Gantry Carriage Bracket:1',
'Right Gantry Carriage Bracket:1','Right Gantry Carriage Bracket:1',#6513,
#6522,'Right Gantry Carriage Bracket:1');
#257=NEXT_ASSEMBLY_USAGE_OCCURRENCE('Bearing Retainer:1',
'Bearing Retainer:1','Bearing Retainer:1',#6513,#6523,
'Bearing Retainer:1');
#258=NEXT_ASSEMBLY_USAGE_OCCURRENCE('Right Gantry Support Bracket:1',
'Right Gantry Support Bracket:1','Right Gantry Support Bracket:1',#6513,
#6524,'Right Gantry Support Bracket:1');
#259=NEXT_ASSEMBLY_USAGE_OCCURRENCE('Linear Motion Ball Bushing:1',
'Linear Motion Ball Bushing:1','Linear Motion Ball Bushing:1',#6514,#6521,
'Linear Motion Ball Bushing:1');
#260=NEXT_ASSEMBLY_USAGE_OCCURRENCE('Right Gantry Carriage Bracket:1',
'Right Gantry Carriage Bracket:1','Right Gantry Carriage Bracket:1',#6514,
#6522,'Right Gantry Carriage Bracket:1');
#261=NEXT_ASSEMBLY_USAGE_OCCURRENCE('Bearing Retainer:1',
'Bearing Retainer:1','Bearing Retainer:1',#6514,#6523,
'Bearing Retainer:1');
#262=NEXT_ASSEMBLY_USAGE_OCCURRENCE('Right Gantry Support Bracket:1',
'Right Gantry Support Bracket:1','Right Gantry Support Bracket:1',#6514,
#6524,'Right Gantry Support Bracket:1');
#263=NEXT_ASSEMBLY_USAGE_OCCURRENCE('Linear Motion Ball Bushing:1',
'Linear Motion Ball Bushing:1','Linear Motion Ball Bushing:1',#6515,#6521,
'Linear Motion Ball Bushing:1');
#264=NEXT_ASSEMBLY_USAGE_OCCURRENCE('Right Gantry Carriage Bracket:1',
'Right Gantry Carriage Bracket:1','Right Gantry Carriage Bracket:1',#6515,
#6522,'Right Gantry Carriage Bracket:1');
#265=NEXT_ASSEMBLY_USAGE_OCCURRENCE('Bearing Retainer:1',
'Bearing Retainer:1','Bearing Retainer:1',#6515,#6523,
'Bearing Retainer:1');
#266=NEXT_ASSEMBLY_USAGE_OCCURRENCE('Right Gantry Support Bracket:1',
'Right Gantry Support Bracket:1','Right Gantry Support Bracket:1',#6515,
#6524,'Right Gantry Support Bracket:1');
#267=NEXT_ASSEMBLY_USAGE_OCCURRENCE('Linear Motion Ball Bushing:1',
'Linear Motion Ball Bushing:1','Linear Motion Ball Bushing:1',#6516,#6521,
'Linear Motion Ball Bushing:1');
#268=NEXT_ASSEMBLY_USAGE_OCCURRENCE('Right Gantry Carriage Bracket:1',
'Right Gantry Carriage Bracket:1','Right Gantry Carriage Bracket:1',#6516,
#6522,'Right Gantry Carriage Bracket:1');
#269=NEXT_ASSEMBLY_USAGE_OCCURRENCE('Bearing Retainer:1',
'Bearing Retainer:1','Bearing Retainer:1',#6516,#6523,
'Bearing Retainer:1');
#270=NEXT_ASSEMBLY_USAGE_OCCURRENCE('Right Gantry Support Bracket:1',
'Right Gantry Support Bracket:1','Right Gantry Support Bracket:1',#6516,
#6524,'Right Gantry Support Bracket:1');
#271=NEXT_ASSEMBLY_USAGE_OCCURRENCE('Linear Motion Ball Bushing:1',
'Linear Motion Ball Bushing:1','Linear Motion Ball Bushing:1',#6517,#6521,
'Linear Motion Ball Bushing:1');
#272=NEXT_ASSEMBLY_USAGE_OCCURRENCE('Right Gantry Carriage Bracket:1',
'Right Gantry Carriage Bracket:1','Right Gantry Carriage Bracket:1',#6517,
#6522,'Right Gantry Carriage Bracket:1');
#273=NEXT_ASSEMBLY_USAGE_OCCURRENCE('Bearing Retainer:1',
'Bearing Retainer:1','Bearing Retainer:1',#6517,#6523,
'Bearing Retainer:1');
#274=NEXT_ASSEMBLY_USAGE_OCCURRENCE('Right Gantry Support Bracket:1',
'Right Gantry Support Bracket:1','Right Gantry Support Bracket:1',#6517,
#6524,'Right Gantry Support Bracket:1');
#275=NEXT_ASSEMBLY_USAGE_OCCURRENCE('Linear Motion Ball Bushing:1',
'Linear Motion Ball Bushing:1','Linear Motion Ball Bushing:1',#6518,#6521,
'Linear Motion Ball Bushing:1');
#276=NEXT_ASSEMBLY_USAGE_OCCURRENCE('Right Gantry Carriage Bracket:1',
'Right Gantry Carriage Bracket:1','Right Gantry Carriage Bracket:1',#6518,
#6522,'Right Gantry Carriage Bracket:1');
#277=NEXT_ASSEMBLY_USAGE_OCCURRENCE('Bearing Retainer:1',
'Bearing Retainer:1','Bearing Retainer:1',#6518,#6523,
'Bearing Retainer:1');
#278=NEXT_ASSEMBLY_USAGE_OCCURRENCE('Right Gantry Support Bracket:1',
'Right Gantry Support Bracket:1','Right Gantry Support Bracket:1',#6518,
#6524,'Right Gantry Support Bracket:1');
#279=NEXT_ASSEMBLY_USAGE_OCCURRENCE('Linear Motion Ball Bushing:1',
'Linear Motion Ball Bushing:1','Linear Motion Ball Bushing:1',#6519,#6521,
'Linear Motion Ball Bushing:1');
#280=NEXT_ASSEMBLY_USAGE_OCCURRENCE('Right Gantry Carriage Bracket:1',
'Right Gantry Carriage Bracket:1','Right Gantry Carriage Bracket:1',#6519,
#6522,'Right Gantry Carriage Bracket:1');
#281=NEXT_ASSEMBLY_USAGE_OCCURRENCE('Bearing Retainer:1',
'Bearing Retainer:1','Bearing Retainer:1',#6519,#6523,
'Bearing Retainer:1');
#282=NEXT_ASSEMBLY_USAGE_OCCURRENCE('Right Gantry Support Bracket:1',
'Right Gantry Support Bracket:1','Right Gantry Support Bracket:1',#6519,
#6524,'Right Gantry Support Bracket:1');
#283=NEXT_ASSEMBLY_USAGE_OCCURRENCE('Linear Motion Ball Bushing:1',
'Linear Motion Ball Bushing:1','Linear Motion Ball Bushing:1',#6520,#6521,
'Linear Motion Ball Bushing:1');
#284=NEXT_ASSEMBLY_USAGE_OCCURRENCE('Right Gantry Carriage Bracket:1',
'Right Gantry Carriage Bracket:1','Right Gantry Carriage Bracket:1',#6520,
#6522,'Right Gantry Carriage Bracket:1');
#285=NEXT_ASSEMBLY_USAGE_OCCURRENCE('Bearing Retainer:1',
'Bearing Retainer:1','Bearing Retainer:1',#6520,#6523,
'Bearing Retainer:1');
#286=NEXT_ASSEMBLY_USAGE_OCCURRENCE('Right Gantry Support Bracket:1',
'Right Gantry Support Bracket:1','Right Gantry Support Bracket:1',#6520,
#6524,'Right Gantry Support Bracket:1');
#287=NEXT_ASSEMBLY_USAGE_OCCURRENCE('Front Right Z Mount:1',
'Front Right Z Mount:1','Front Right Z Mount:1',#6501,#6502,
'Front Right Z Mount:1');
#288=NEXT_ASSEMBLY_USAGE_OCCURRENCE('Back Left Z Mount:1',
'Back Left Z Mount:1','Back Left Z Mount:1',#6501,#6503,
'Back Left Z Mount:1');
#289=NEXT_ASSEMBLY_USAGE_OCCURRENCE('Front Left Z Mount:1',
'Front Left Z Mount:1','Front Left Z Mount:1',#6501,#6504,
'Front Left Z Mount:1');
#290=NEXT_ASSEMBLY_USAGE_OCCURRENCE('Back Right Z Mount:1',
'Back Right Z Mount:1','Back Right Z Mount:1',#6501,#6505,
'Back Right Z Mount:1');
#291=NEXT_ASSEMBLY_USAGE_OCCURRENCE('Linear Bearing Assembly:1',
'Linear Bearing Assembly:1','Linear Bearing Assembly:1',#6501,#6506,
'Linear Bearing Assembly:1');
#292=NEXT_ASSEMBLY_USAGE_OCCURRENCE('8mm Z Axis Rod:1',
'8mm Z Axis Rod:1','8mm Z Axis Rod:1',#6501,#6509,'8mm Z Axis Rod:1');
#293=NEXT_ASSEMBLY_USAGE_OCCURRENCE('8mm Z Axis Rod:2',
'8mm Z Axis Rod:2','8mm Z Axis Rod:2',#6501,#6509,'8mm Z Axis Rod:2');
#294=NEXT_ASSEMBLY_USAGE_OCCURRENCE('8mm Z Axis Rod:3',
'8mm Z Axis Rod:3','8mm Z Axis Rod:3',#6501,#6509,'8mm Z Axis Rod:3');
#295=NEXT_ASSEMBLY_USAGE_OCCURRENCE('8mm Z Axis Rod:6',
'8mm Z Axis Rod:6','8mm Z Axis Rod:6',#6501,#6509,'8mm Z Axis Rod:6');
#296=NEXT_ASSEMBLY_USAGE_OCCURRENCE('8mm Z Axis Rod:7',
'8mm Z Axis Rod:7','8mm Z Axis Rod:7',#6501,#6509,'8mm Z Axis Rod:7');
#297=NEXT_ASSEMBLY_USAGE_OCCURRENCE('8mm Z Axis Rod:9',
'8mm Z Axis Rod:9','8mm Z Axis Rod:9',#6501,#6509,'8mm Z Axis Rod:9');
#298=NEXT_ASSEMBLY_USAGE_OCCURRENCE('8mm Z Axis Rod:10',
'8mm Z Axis Rod:10','8mm Z Axis Rod:10',#6501,#6509,'8mm Z Axis Rod:10');
#299=NEXT_ASSEMBLY_USAGE_OCCURRENCE('End Cap Right:1','End Cap Right:1',
'End Cap Right:1',#6501,#6507,'End Cap Right:1');
#300=NEXT_ASSEMBLY_USAGE_OCCURRENCE('End Cap Left:1','End Cap Left:1',
'End Cap Left:1',#6501,#6508,'End Cap Left:1');
#301=NEXT_ASSEMBLY_USAGE_OCCURRENCE('8mm Z Axis Rod:4',
'8mm Z Axis Rod:4','8mm Z Axis Rod:4',#6501,#6509,'8mm Z Axis Rod:4');
#302=NEXT_ASSEMBLY_USAGE_OCCURRENCE('8mm Z Axis Rod:8',
'8mm Z Axis Rod:8','8mm Z Axis Rod:8',#6501,#6509,'8mm Z Axis Rod:8');
#303=NEXT_ASSEMBLY_USAGE_OCCURRENCE('8mm Z Axis Rod:5',
'8mm Z Axis Rod:5','8mm Z Axis Rod:5',#6501,#6509,'8mm Z Axis Rod:5');
#304=NEXT_ASSEMBLY_USAGE_OCCURRENCE('Linear Bearing Assembly:2',
'Linear Bearing Assembly:2','Linear Bearing Assembly:2',#6501,#6510,
'Linear Bearing Assembly:2');
#305=NEXT_ASSEMBLY_USAGE_OCCURRENCE('Linear Bearing Assembly:3',
'Linear Bearing Assembly:3','Linear Bearing Assembly:3',#6501,#6511,
'Linear Bearing Assembly:3');
#306=NEXT_ASSEMBLY_USAGE_OCCURRENCE('Linear Bearing Assembly:4',
'Linear Bearing Assembly:4','Linear Bearing Assembly:4',#6501,#6512,
'Linear Bearing Assembly:4');
#307=NEXT_ASSEMBLY_USAGE_OCCURRENCE('Linear Bearing Assembly:5',
'Linear Bearing Assembly:5','Linear Bearing Assembly:5',#6501,#6513,
'Linear Bearing Assembly:5');
#308=NEXT_ASSEMBLY_USAGE_OCCURRENCE('Linear Bearing Assembly:6',
'Linear Bearing Assembly:6','Linear Bearing Assembly:6',#6501,#6514,
'Linear Bearing Assembly:6');
#309=NEXT_ASSEMBLY_USAGE_OCCURRENCE('Linear Bearing Assembly:7',
'Linear Bearing Assembly:7','Linear Bearing Assembly:7',#6501,#6515,
'Linear Bearing Assembly:7');
#310=NEXT_ASSEMBLY_USAGE_OCCURRENCE('Linear Bearing Assembly:8',
'Linear Bearing Assembly:8','Linear Bearing Assembly:8',#6501,#6516,
'Linear Bearing Assembly:8');
#311=NEXT_ASSEMBLY_USAGE_OCCURRENCE('Linear Bearing Assembly:9',
'Linear Bearing Assembly:9','Linear Bearing Assembly:9',#6501,#6517,
'Linear Bearing Assembly:9');
#312=NEXT_ASSEMBLY_USAGE_OCCURRENCE('Linear Bearing Assembly:10',
'Linear Bearing Assembly:10','Linear Bearing Assembly:10',#6501,#6518,
'Linear Bearing Assembly:10');
#313=NEXT_ASSEMBLY_USAGE_OCCURRENCE('Linear Bearing Assembly:11',
'Linear Bearing Assembly:11','Linear Bearing Assembly:11',#6501,#6519,
'Linear Bearing Assembly:11');
#314=NEXT_ASSEMBLY_USAGE_OCCURRENCE('Linear Bearing Assembly:12',
'Linear Bearing Assembly:12','Linear Bearing Assembly:12',#6501,#6520,
'Linear Bearing Assembly:12');
#315=CONICAL_SURFACE('',#3805,0.0066,0.785398163397459);
#316=CONICAL_SURFACE('',#3813,0.0074,0.785398163397448);
#317=CONICAL_SURFACE('',#3818,0.0066,0.785398163397459);
#318=CONICAL_SURFACE('',#3826,0.0074,0.785398163397448);
#319=CONICAL_SURFACE('',#3839,0.0061,0.158655262186402);
#320=CONICAL_SURFACE('',#3843,0.0061,0.158655262186402);
#321=CONICAL_SURFACE('',#3873,0.0043,0.785398163397448);
#322=CONICAL_SURFACE('',#3879,0.0046499998960644,0.785398163397448);
#323=CONICAL_SURFACE('',#3888,0.0043,0.785398163397448);
#324=CONICAL_SURFACE('',#3894,0.0046499998960644,0.785398163397448);
#325=TOROIDAL_SURFACE('',#3789,0.0025,0.0015);
#326=TOROIDAL_SURFACE('',#3791,0.0025,0.0015);
#327=SHAPE_REPRESENTATION_RELATIONSHIP('SRR','None',#6477,#338);
#328=SHAPE_REPRESENTATION_RELATIONSHIP('SRR','None',#6478,#339);
#329=SHAPE_REPRESENTATION_RELATIONSHIP('SRR','None',#6479,#340);
#330=SHAPE_REPRESENTATION_RELATIONSHIP('SRR','None',#6480,#341);
#331=SHAPE_REPRESENTATION_RELATIONSHIP('SRR','None',#6482,#342);
#332=SHAPE_REPRESENTATION_RELATIONSHIP('SRR','None',#6483,#343);
#333=SHAPE_REPRESENTATION_RELATIONSHIP('SRR','None',#6484,#344);
#334=SHAPE_REPRESENTATION_RELATIONSHIP('SRR','None',#6496,#345);
#335=SHAPE_REPRESENTATION_RELATIONSHIP('SRR','None',#6497,#346);
#336=SHAPE_REPRESENTATION_RELATIONSHIP('SRR','None',#6498,#347);
#337=SHAPE_REPRESENTATION_RELATIONSHIP('SRR','None',#6499,#348);
#338=ADVANCED_BREP_SHAPE_REPRESENTATION('',(#360),#6325);
#339=ADVANCED_BREP_SHAPE_REPRESENTATION('',(#361),#6326);
#340=ADVANCED_BREP_SHAPE_REPRESENTATION('',(#362),#6327);
#341=ADVANCED_BREP_SHAPE_REPRESENTATION('',(#363),#6328);
#342=ADVANCED_BREP_SHAPE_REPRESENTATION('',(#364),#6330);
#343=ADVANCED_BREP_SHAPE_REPRESENTATION('',(#365),#6331);
#344=ADVANCED_BREP_SHAPE_REPRESENTATION('',(#366),#6332);
#345=ADVANCED_BREP_SHAPE_REPRESENTATION('',(#367),#6344);
#346=ADVANCED_BREP_SHAPE_REPRESENTATION('',(#368),#6345);
#347=ADVANCED_BREP_SHAPE_REPRESENTATION('',(#369),#6346);
#348=ADVANCED_BREP_SHAPE_REPRESENTATION('',(#370),#6347);
#349=STYLED_ITEM('',(#6601),#360);
#350=STYLED_ITEM('',(#6602),#361);
#351=STYLED_ITEM('',(#6602),#362);
#352=STYLED_ITEM('',(#6601),#363);
#353=STYLED_ITEM('',(#6603),#364);
#354=STYLED_ITEM('',(#6604),#365);
#355=STYLED_ITEM('',(#6605),#366);
#356=STYLED_ITEM('',(#6603),#367);
#357=STYLED_ITEM('',(#6604),#368);
#358=STYLED_ITEM('',(#6604),#369);
#359=STYLED_ITEM('',(#6603),#370);
#360=MANIFOLD_SOLID_BREP('Body1',#3388);
#361=MANIFOLD_SOLID_BREP('Body1',#3389);
#362=MANIFOLD_SOLID_BREP('Body1',#3390);
#363=MANIFOLD_SOLID_BREP('Body1',#3391);
#364=MANIFOLD_SOLID_BREP('Body1',#3392);
#365=MANIFOLD_SOLID_BREP('Body1',#3393);
#366=MANIFOLD_SOLID_BREP('Body1',#3394);
#367=MANIFOLD_SOLID_BREP('Body1',#3395);
#368=MANIFOLD_SOLID_BREP('Body1',#3396);
#369=MANIFOLD_SOLID_BREP('Body1',#3397);
#370=MANIFOLD_SOLID_BREP('Body1',#3398);
#371=B_SPLINE_CURVE_WITH_KNOTS('',3,(#5227,#5228,#5229,#5230,#5231,#5232,
#5233,#5234,#5235,#5236,#5237,#5238,#5239,#5240,#5241,#5242,#5243,#5244),
 .UNSPECIFIED.,.F.,.F.,(4,2,2,2,2,2,2,2,4),(3.70111917994048,3.77979672158967,
4.08163951097076,4.2325609056613,4.38348230035184,4.53440369504239,4.68532508973293,
4.98716787911402,5.06584542076321),.UNSPECIFIED.);
#372=B_SPLINE_CURVE_WITH_KNOTS('',3,(#5245,#5246,#5247,#5248,#5249,#5250,
#5251,#5252,#5253,#5254,#5255,#5256,#5257,#5258,#5259,#5260,#5261,#5262),
 .UNSPECIFIED.,.F.,.F.,(4,2,2,2,2,2,2,2,4),(0.778797646372586,0.857475188021775,
1.15931797740286,1.31023937209341,1.46116076678395,1.61208216147449,1.76300355616504,
2.06484634554612,2.14352388719531),.UNSPECIFIED.);
#373=B_SPLINE_CURVE_WITH_KNOTS('',3,(#5376,#5377,#5378,#5379,#5380,#5381,
#5382,#5383,#5384,#5385,#5386,#5387,#5388,#5389,#5390,#5391,#5392,#5393),
 .UNSPECIFIED.,.F.,.F.,(4,2,2,2,2,2,2,2,4),(3.70111917994048,3.77979672158967,
4.08163951097076,4.2325609056613,4.38348230035184,4.53440369504239,4.68532508973293,
4.98716787911402,5.06584542076321),.UNSPECIFIED.);
#374=B_SPLINE_CURVE_WITH_KNOTS('',3,(#5394,#5395,#5396,#5397,#5398,#5399,
#5400,#5401,#5402,#5403,#5404,#5405,#5406,#5407,#5408,#5409,#5410,#5411),
 .UNSPECIFIED.,.F.,.F.,(4,2,2,2,2,2,2,2,4),(0.778797646372586,0.857475188021775,
1.15931797740286,1.31023937209341,1.46116076678395,1.61208216147449,1.76300355616504,
2.06484634554612,2.14352388719531),.UNSPECIFIED.);
#375=B_SPLINE_CURVE_WITH_KNOTS('',3,(#5524,#5525,#5526,#5527,#5528,#5529,
#5530,#5531,#5532,#5533,#5534,#5535,#5536,#5537,#5538,#5539,#5540,#5541),
 .UNSPECIFIED.,.F.,.F.,(4,2,2,2,2,2,2,2,4),(-2.14352388719531,-2.06484634554612,
-1.76300355616504,-1.61208216147449,-1.46116076678395,-1.31023937209341,
-1.15931797740286,-0.857475188021775,-0.778797646372586),.UNSPECIFIED.);
#376=B_SPLINE_CURVE_WITH_KNOTS('',3,(#5543,#5544,#5545,#5546,#5547,#5548,
#5549,#5550,#5551,#5552,#5553,#5554,#5555,#5556,#5557,#5558,#5559,#5560),
 .UNSPECIFIED.,.F.,.F.,(4,2,2,2,2,2,2,2,4),(-5.06584542076321,-4.98716787911402,
-4.68532508973293,-4.53440369504239,-4.38348230035184,-4.2325609056613,
-4.08163951097076,-3.77979672158967,-3.70111917994048),.UNSPECIFIED.);
#377=B_SPLINE_CURVE_WITH_KNOTS('',3,(#5673,#5674,#5675,#5676,#5677,#5678,
#5679,#5680,#5681,#5682,#5683,#5684,#5685,#5686,#5687,#5688,#5689,#5690),
 .UNSPECIFIED.,.F.,.F.,(4,2,2,2,2,2,2,2,4),(-2.14352388719531,-2.06484634554612,
-1.76300355616504,-1.61208216147449,-1.46116076678395,-1.31023937209341,
-1.15931797740286,-0.857475188021775,-0.778797646372586),.UNSPECIFIED.);
#378=B_SPLINE_CURVE_WITH_KNOTS('',3,(#5692,#5693,#5694,#5695,#5696,#5697,
#5698,#5699,#5700,#5701,#5702,#5703,#5704,#5705,#5706,#5707,#5708,#5709),
 .UNSPECIFIED.,.F.,.F.,(4,2,2,2,2,2,2,2,4),(-5.06584542076321,-4.98716787911402,
-4.68532508973293,-4.53440369504239,-4.38348230035184,-4.2325609056613,
-4.08163951097076,-3.77979672158967,-3.70111917994048),.UNSPECIFIED.);
#379=B_SPLINE_CURVE_WITH_KNOTS('',3,(#5841,#5842,#5843,#5844,#5845,#5846),
 .UNSPECIFIED.,.F.,.F.,(4,2,4),(3.46797062946804,3.66737221611079,3.95578831781598),
 .UNSPECIFIED.);
#380=B_SPLINE_CURVE_WITH_KNOTS('',3,(#5847,#5848,#5849,#5850,#5851,#5852),
 .UNSPECIFIED.,.F.,.F.,(4,2,4),(3.95578831781598,4.24420441952117,4.44360600616391),
 .UNSPECIFIED.);
#381=B_SPLINE_CURVE_WITH_KNOTS('',3,(#5855,#5856,#5857,#5858,#5859,#5860,
#5861,#5862,#5863,#5864),.UNSPECIFIED.,.F.,.F.,(4,2,2,2,4),(3.46797062946804,
3.66737221611078,3.95578831781597,4.24420441952117,4.44360600616391),
 .UNSPECIFIED.);
#382=B_SPLINE_CURVE_WITH_KNOTS('',3,(#5983,#5984,#5985,#5986,#5987,#5988),
 .UNSPECIFIED.,.F.,.F.,(4,2,4),(3.46797062946804,3.66737221611079,3.95578831781598),
 .UNSPECIFIED.);
#383=B_SPLINE_CURVE_WITH_KNOTS('',3,(#5989,#5990,#5991,#5992,#5993,#5994),
 .UNSPECIFIED.,.F.,.F.,(4,2,4),(3.95578831781598,4.24420441952117,4.44360600616391),
 .UNSPECIFIED.);
#384=B_SPLINE_CURVE_WITH_KNOTS('',3,(#5997,#5998,#5999,#6000,#6001,#6002,
#6003,#6004,#6005,#6006),.UNSPECIFIED.,.F.,.F.,(4,2,2,2,4),(-4.44360600616391,
-4.24420441952117,-3.95578831781597,-3.66737221611078,-3.46797062946804),
 .UNSPECIFIED.);
#385=CYLINDRICAL_SURFACE('',#3548,0.004225);
#386=CYLINDRICAL_SURFACE('',#3549,0.004225);
#387=CYLINDRICAL_SURFACE('',#3551,0.0075);
#388=CYLINDRICAL_SURFACE('',#3556,0.005);
#389=CYLINDRICAL_SURFACE('',#3557,0.005);
#390=CYLINDRICAL_SURFACE('',#3558,0.005);
#391=CYLINDRICAL_SURFACE('',#3559,0.005);
#392=CYLINDRICAL_SURFACE('',#3560,0.005);
#393=CYLINDRICAL_SURFACE('',#3561,0.005);
#394=CYLINDRICAL_SURFACE('',#3588,0.004225);
#395=CYLINDRICAL_SURFACE('',#3589,0.004225);
#396=CYLINDRICAL_SURFACE('',#3591,0.0075);
#397=CYLINDRICAL_SURFACE('',#3596,0.005);
#398=CYLINDRICAL_SURFACE('',#3597,0.005);
#399=CYLINDRICAL_SURFACE('',#3598,0.005);
#400=CYLINDRICAL_SURFACE('',#3599,0.005);
#401=CYLINDRICAL_SURFACE('',#3600,0.005);
#402=CYLINDRICAL_SURFACE('',#3601,0.005);
#403=CYLINDRICAL_SURFACE('',#3628,0.004225);
#404=CYLINDRICAL_SURFACE('',#3629,0.004225);
#405=CYLINDRICAL_SURFACE('',#3631,0.0075);
#406=CYLINDRICAL_SURFACE('',#3636,0.005);
#407=CYLINDRICAL_SURFACE('',#3637,0.005);
#408=CYLINDRICAL_SURFACE('',#3638,0.005);
#409=CYLINDRICAL_SURFACE('',#3639,0.005);
#410=CYLINDRICAL_SURFACE('',#3640,0.005);
#411=CYLINDRICAL_SURFACE('',#3641,0.005);
#412=CYLINDRICAL_SURFACE('',#3668,0.004225);
#413=CYLINDRICAL_SURFACE('',#3669,0.004225);
#414=CYLINDRICAL_SURFACE('',#3671,0.0075);
#415=CYLINDRICAL_SURFACE('',#3676,0.005);
#416=CYLINDRICAL_SURFACE('',#3677,0.005);
#417=CYLINDRICAL_SURFACE('',#3678,0.005);
#418=CYLINDRICAL_SURFACE('',#3679,0.005);
#419=CYLINDRICAL_SURFACE('',#3680,0.005);
#420=CYLINDRICAL_SURFACE('',#3681,0.005);
#421=CYLINDRICAL_SURFACE('',#3690,0.004225);
#422=CYLINDRICAL_SURFACE('',#3694,0.004225);
#423=CYLINDRICAL_SURFACE('',#3717,0.005);
#424=CYLINDRICAL_SURFACE('',#3718,0.005);
#425=CYLINDRICAL_SURFACE('',#3719,0.005);
#426=CYLINDRICAL_SURFACE('',#3720,0.005);
#427=CYLINDRICAL_SURFACE('',#3725,0.007625);
#428=CYLINDRICAL_SURFACE('',#3726,0.007625);
#429=CYLINDRICAL_SURFACE('',#3727,0.005);
#430=CYLINDRICAL_SURFACE('',#3728,0.005);
#431=CYLINDRICAL_SURFACE('',#3729,0.005);
#432=CYLINDRICAL_SURFACE('',#3730,0.005);
#433=CYLINDRICAL_SURFACE('',#3738,0.004225);
#434=CYLINDRICAL_SURFACE('',#3742,0.004225);
#435=CYLINDRICAL_SURFACE('',#3765,0.005);
#436=CYLINDRICAL_SURFACE('',#3766,0.005);
#437=CYLINDRICAL_SURFACE('',#3767,0.005);
#438=CYLINDRICAL_SURFACE('',#3768,0.005);
#439=CYLINDRICAL_SURFACE('',#3773,0.007625);
#440=CYLINDRICAL_SURFACE('',#3774,0.007625);
#441=CYLINDRICAL_SURFACE('',#3775,0.005);
#442=CYLINDRICAL_SURFACE('',#3776,0.005);
#443=CYLINDRICAL_SURFACE('',#3777,0.005);
#444=CYLINDRICAL_SURFACE('',#3778,0.005);
#445=CYLINDRICAL_SURFACE('',#3780,0.004);
#446=CYLINDRICAL_SURFACE('',#3811,0.0065);
#447=CYLINDRICAL_SURFACE('',#3816,0.0075);
#448=CYLINDRICAL_SURFACE('',#3824,0.0065);
#449=CYLINDRICAL_SURFACE('',#3829,0.0075);
#450=CYLINDRICAL_SURFACE('',#3833,0.00700000010430813);
#451=CYLINDRICAL_SURFACE('',#3837,0.0063);
#452=CYLINDRICAL_SURFACE('',#3841,0.0059);
#453=CYLINDRICAL_SURFACE('',#3845,0.0063);
#454=CYLINDRICAL_SURFACE('',#3849,0.00700000010430813);
#455=CYLINDRICAL_SURFACE('',#3854,0.00715);
#456=CYLINDRICAL_SURFACE('',#3858,0.0075);
#457=CYLINDRICAL_SURFACE('',#3862,0.00715);
#458=CYLINDRICAL_SURFACE('',#3869,0.0065);
#459=CYLINDRICAL_SURFACE('',#3875,0.00405);
#460=CYLINDRICAL_SURFACE('',#3884,0.0065);
#461=CYLINDRICAL_SURFACE('',#3890,0.00405);
#462=CYLINDRICAL_SURFACE('',#3899,0.007);
#463=CYLINDRICAL_SURFACE('',#3903,0.0043);
#464=FACE_BOUND('',#869,.T.);
#465=FACE_BOUND('',#870,.T.);
#466=FACE_BOUND('',#872,.T.);
#467=FACE_BOUND('',#873,.T.);
#468=FACE_BOUND('',#892,.T.);
#469=FACE_BOUND('',#893,.T.);
#470=FACE_BOUND('',#895,.T.);
#471=FACE_BOUND('',#896,.T.);
#472=FACE_BOUND('',#915,.T.);
#473=FACE_BOUND('',#916,.T.);
#474=FACE_BOUND('',#918,.T.);
#475=FACE_BOUND('',#919,.T.);
#476=FACE_BOUND('',#938,.T.);
#477=FACE_BOUND('',#939,.T.);
#478=FACE_BOUND('',#941,.T.);
#479=FACE_BOUND('',#942,.T.);
#480=FACE_BOUND('',#960,.T.);
#481=FACE_BOUND('',#961,.T.);
#482=FACE_BOUND('',#967,.T.);
#483=FACE_BOUND('',#968,.T.);
#484=FACE_BOUND('',#986,.T.);
#485=FACE_BOUND('',#987,.T.);
#486=FACE_BOUND('',#993,.T.);
#487=FACE_BOUND('',#994,.T.);
#488=FACE_BOUND('',#1016,.T.);
#489=FACE_BOUND('',#1022,.T.);
#490=FACE_BOUND('',#1027,.T.);
#491=FACE_BOUND('',#1030,.T.);
#492=FACE_BOUND('',#1037,.T.);
#493=FACE_BOUND('',#1040,.T.);
#494=FACE_BOUND('',#1042,.T.);
#495=FACE_BOUND('',#1045,.T.);
#496=FACE_BOUND('',#1048,.T.);
#497=FACE_BOUND('',#1051,.T.);
#498=FACE_BOUND('',#1053,.T.);
#499=FACE_BOUND('',#1056,.T.);
#500=FACE_BOUND('',#1060,.T.);
#501=FACE_BOUND('',#1063,.T.);
#502=FACE_BOUND('',#1066,.T.);
#503=FACE_BOUND('',#1070,.T.);
#504=FACE_BOUND('',#1073,.T.);
#505=FACE_BOUND('',#1076,.T.);
#506=CIRCLE('',#3525,0.0075);
#507=CIRCLE('',#3526,0.0075);
#508=CIRCLE('',#3528,0.0075);
#509=CIRCLE('',#3529,0.0075);
#510=CIRCLE('',#3531,0.005);
#511=CIRCLE('',#3532,0.005);
#512=CIRCLE('',#3533,0.005);
#513=CIRCLE('',#3534,0.005);
#514=CIRCLE('',#3535,0.005);
#515=CIRCLE('',#3536,0.005);
#516=CIRCLE('',#3537,0.004225);
#517=CIRCLE('',#3538,0.004225);
#518=CIRCLE('',#3540,0.005);
#519=CIRCLE('',#3541,0.005);
#520=CIRCLE('',#3542,0.005);
#521=CIRCLE('',#3543,0.005);
#522=CIRCLE('',#3544,0.005);
#523=CIRCLE('',#3545,0.005);
#524=CIRCLE('',#3546,0.004225);
#525=CIRCLE('',#3547,0.004225);
#526=CIRCLE('',#3565,0.0075);
#527=CIRCLE('',#3566,0.0075);
#528=CIRCLE('',#3568,0.0075);
#529=CIRCLE('',#3569,0.0075);
#530=CIRCLE('',#3571,0.005);
#531=CIRCLE('',#3572,0.005);
#532=CIRCLE('',#3573,0.005);
#533=CIRCLE('',#3574,0.005);
#534=CIRCLE('',#3575,0.005);
#535=CIRCLE('',#3576,0.005);
#536=CIRCLE('',#3577,0.004225);
#537=CIRCLE('',#3578,0.004225);
#538=CIRCLE('',#3580,0.005);
#539=CIRCLE('',#3581,0.005);
#540=CIRCLE('',#3582,0.005);
#541=CIRCLE('',#3583,0.005);
#542=CIRCLE('',#3584,0.005);
#543=CIRCLE('',#3585,0.005);
#544=CIRCLE('',#3586,0.004225);
#545=CIRCLE('',#3587,0.004225);
#546=CIRCLE('',#3605,0.0075);
#547=CIRCLE('',#3606,0.0075);
#548=CIRCLE('',#3608,0.0075);
#549=CIRCLE('',#3609,0.0075);
#550=CIRCLE('',#3611,0.005);
#551=CIRCLE('',#3612,0.005);
#552=CIRCLE('',#3613,0.005);
#553=CIRCLE('',#3614,0.005);
#554=CIRCLE('',#3615,0.005);
#555=CIRCLE('',#3616,0.005);
#556=CIRCLE('',#3617,0.004225);
#557=CIRCLE('',#3618,0.004225);
#558=CIRCLE('',#3620,0.005);
#559=CIRCLE('',#3621,0.005);
#560=CIRCLE('',#3622,0.005);
#561=CIRCLE('',#3623,0.005);
#562=CIRCLE('',#3624,0.005);
#563=CIRCLE('',#3625,0.005);
#564=CIRCLE('',#3626,0.004225);
#565=CIRCLE('',#3627,0.004225);
#566=CIRCLE('',#3645,0.0075);
#567=CIRCLE('',#3646,0.0075);
#568=CIRCLE('',#3648,0.0075);
#569=CIRCLE('',#3649,0.0075);
#570=CIRCLE('',#3651,0.005);
#571=CIRCLE('',#3652,0.005);
#572=CIRCLE('',#3653,0.005);
#573=CIRCLE('',#3654,0.005);
#574=CIRCLE('',#3655,0.005);
#575=CIRCLE('',#3656,0.005);
#576=CIRCLE('',#3657,0.004225);
#577=CIRCLE('',#3658,0.004225);
#578=CIRCLE('',#3660,0.005);
#579=CIRCLE('',#3661,0.005);
#580=CIRCLE('',#3662,0.005);
#581=CIRCLE('',#3663,0.005);
#582=CIRCLE('',#3664,0.005);
#583=CIRCLE('',#3665,0.005);
#584=CIRCLE('',#3666,0.004225);
#585=CIRCLE('',#3667,0.004225);
#586=CIRCLE('',#3687,0.007625);
#587=CIRCLE('',#3688,0.007625);
#588=CIRCLE('',#3691,0.004225);
#589=CIRCLE('',#3692,0.004225);
#590=CIRCLE('',#3695,0.004225);
#591=CIRCLE('',#3696,0.004225);
#592=CIRCLE('',#3698,0.005);
#593=CIRCLE('',#3699,0.005);
#594=CIRCLE('',#3700,0.005);
#595=CIRCLE('',#3701,0.005);
#596=CIRCLE('',#3702,0.005);
#597=CIRCLE('',#3703,0.005);
#598=CIRCLE('',#3704,0.005);
#599=CIRCLE('',#3705,0.005);
#600=CIRCLE('',#3709,0.005);
#601=CIRCLE('',#3710,0.005);
#602=CIRCLE('',#3711,0.005);
#603=CIRCLE('',#3712,0.005);
#604=CIRCLE('',#3713,0.005);
#605=CIRCLE('',#3714,0.005);
#606=CIRCLE('',#3715,0.005);
#607=CIRCLE('',#3716,0.005);
#608=CIRCLE('',#3722,0.007625);
#609=CIRCLE('',#3723,0.007625);
#610=CIRCLE('',#3724,0.007625);
#611=CIRCLE('',#3735,0.007625);
#612=CIRCLE('',#3736,0.007625);
#613=CIRCLE('',#3739,0.004225);
#614=CIRCLE('',#3740,0.004225);
#615=CIRCLE('',#3743,0.004225);
#616=CIRCLE('',#3744,0.004225);
#617=CIRCLE('',#3746,0.005);
#618=CIRCLE('',#3747,0.005);
#619=CIRCLE('',#3748,0.005);
#620=CIRCLE('',#3749,0.005);
#621=CIRCLE('',#3750,0.005);
#622=CIRCLE('',#3751,0.005);
#623=CIRCLE('',#3752,0.005);
#624=CIRCLE('',#3753,0.005);
#625=CIRCLE('',#3757,0.005);
#626=CIRCLE('',#3758,0.005);
#627=CIRCLE('',#3759,0.005);
#628=CIRCLE('',#3760,0.005);
#629=CIRCLE('',#3761,0.005);
#630=CIRCLE('',#3762,0.005);
#631=CIRCLE('',#3763,0.005);
#632=CIRCLE('',#3764,0.005);
#633=CIRCLE('',#3770,0.007625);
#634=CIRCLE('',#3771,0.007625);
#635=CIRCLE('',#3772,0.007625);
#636=CIRCLE('',#3781,0.004);
#637=CIRCLE('',#3782,0.004);
#638=CIRCLE('',#3783,0.004);
#639=CIRCLE('',#3784,0.004);
#640=CIRCLE('',#3786,0.0025);
#641=CIRCLE('',#3788,0.0025);
#642=CIRCLE('',#3790,0.0015);
#643=CIRCLE('',#3792,0.0015);
#644=CIRCLE('',#3806,0.00650000000001);
#645=CIRCLE('',#3807,0.00670000000001);
#646=CIRCLE('',#3808,0.00650000000001);
#647=CIRCLE('',#3810,0.00730000000001);
#648=CIRCLE('',#3812,0.00650000000001);
#649=CIRCLE('',#3814,0.00750000000001);
#650=CIRCLE('',#3815,0.00750000000001);
#651=CIRCLE('',#3817,0.00750000000001);
#652=CIRCLE('',#3819,0.00650000000001);
#653=CIRCLE('',#3820,0.00670000000001);
#654=CIRCLE('',#3821,0.00650000000001);
#655=CIRCLE('',#3823,0.00730000000001);
#656=CIRCLE('',#3825,0.00650000000001);
#657=CIRCLE('',#3827,0.00750000000001);
#658=CIRCLE('',#3828,0.00750000000001);
#659=CIRCLE('',#3830,0.00750000000001);
#660=CIRCLE('',#3832,0.00700000010431813);
#661=CIRCLE('',#3834,0.00700000010431813);
#662=CIRCLE('',#3836,0.00630000000001);
#663=CIRCLE('',#3838,0.00630000000001);
#664=CIRCLE('',#3840,0.00590000000001);
#665=CIRCLE('',#3842,0.00590000000001);
#666=CIRCLE('',#3844,0.00630000000001);
#667=CIRCLE('',#3846,0.00630000000001);
#668=CIRCLE('',#3848,0.00700000010431813);
#669=CIRCLE('',#3850,0.00700000010431813);
#670=CIRCLE('',#3853,0.00715000000001);
#671=CIRCLE('',#3855,0.00715000000001);
#672=CIRCLE('',#3857,0.00750000000001);
#673=CIRCLE('',#3859,0.00750000000001);
#674=CIRCLE('',#3861,0.00715000000001);
#675=CIRCLE('',#3863,0.00715000000001);
#676=CIRCLE('',#3867,0.00650000000001);
#677=CIRCLE('',#3868,0.00479999989272164);
#678=CIRCLE('',#3870,0.00650000000001);
#679=CIRCLE('',#3872,0.00455000000001);
#680=CIRCLE('',#3874,0.00405000000001);
#681=CIRCLE('',#3876,0.00405000000001);
#682=CIRCLE('',#3878,0.00449999989942716);
#683=CIRCLE('',#3882,0.00650000000001);
#684=CIRCLE('',#3883,0.00479999989272164);
#685=CIRCLE('',#3885,0.00650000000001);
#686=CIRCLE('',#3887,0.00455000000001);
#687=CIRCLE('',#3889,0.00405000000001);
#688=CIRCLE('',#3891,0.00405000000001);
#689=CIRCLE('',#3893,0.00449999989942716);
#690=CIRCLE('',#3897,0.00700000000001);
#691=CIRCLE('',#3898,0.00430000000001);
#692=CIRCLE('',#3900,0.00700000000001);
#693=CIRCLE('',#3902,0.00430000000001);
#694=FACE_OUTER_BOUND('',#865,.T.);
#695=FACE_OUTER_BOUND('',#866,.T.);
#696=FACE_OUTER_BOUND('',#867,.T.);
#697=FACE_OUTER_BOUND('',#868,.T.);
#698=FACE_OUTER_BOUND('',#871,.T.);
#699=FACE_OUTER_BOUND('',#874,.T.);
#700=FACE_OUTER_BOUND('',#875,.T.);
#701=FACE_OUTER_BOUND('',#876,.T.);
#702=FACE_OUTER_BOUND('',#877,.T.);
#703=FACE_OUTER_BOUND('',#878,.T.);
#704=FACE_OUTER_BOUND('',#879,.T.);
#705=FACE_OUTER_BOUND('',#880,.T.);
#706=FACE_OUTER_BOUND('',#881,.T.);
#707=FACE_OUTER_BOUND('',#882,.T.);
#708=FACE_OUTER_BOUND('',#883,.T.);
#709=FACE_OUTER_BOUND('',#884,.T.);
#710=FACE_OUTER_BOUND('',#885,.T.);
#711=FACE_OUTER_BOUND('',#886,.T.);
#712=FACE_OUTER_BOUND('',#887,.T.);
#713=FACE_OUTER_BOUND('',#888,.T.);
#714=FACE_OUTER_BOUND('',#889,.T.);
#715=FACE_OUTER_BOUND('',#890,.T.);
#716=FACE_OUTER_BOUND('',#891,.T.);
#717=FACE_OUTER_BOUND('',#894,.T.);
#718=FACE_OUTER_BOUND('',#897,.T.);
#719=FACE_OUTER_BOUND('',#898,.T.);
#720=FACE_OUTER_BOUND('',#899,.T.);
#721=FACE_OUTER_BOUND('',#900,.T.);
#722=FACE_OUTER_BOUND('',#901,.T.);
#723=FACE_OUTER_BOUND('',#902,.T.);
#724=FACE_OUTER_BOUND('',#903,.T.);
#725=FACE_OUTER_BOUND('',#904,.T.);
#726=FACE_OUTER_BOUND('',#905,.T.);
#727=FACE_OUTER_BOUND('',#906,.T.);
#728=FACE_OUTER_BOUND('',#907,.T.);
#729=FACE_OUTER_BOUND('',#908,.T.);
#730=FACE_OUTER_BOUND('',#909,.T.);
#731=FACE_OUTER_BOUND('',#910,.T.);
#732=FACE_OUTER_BOUND('',#911,.T.);
#733=FACE_OUTER_BOUND('',#912,.T.);
#734=FACE_OUTER_BOUND('',#913,.T.);
#735=FACE_OUTER_BOUND('',#914,.T.);
#736=FACE_OUTER_BOUND('',#917,.T.);
#737=FACE_OUTER_BOUND('',#920,.T.);
#738=FACE_OUTER_BOUND('',#921,.T.);
#739=FACE_OUTER_BOUND('',#922,.T.);
#740=FACE_OUTER_BOUND('',#923,.T.);
#741=FACE_OUTER_BOUND('',#924,.T.);
#742=FACE_OUTER_BOUND('',#925,.T.);
#743=FACE_OUTER_BOUND('',#926,.T.);
#744=FACE_OUTER_BOUND('',#927,.T.);
#745=FACE_OUTER_BOUND('',#928,.T.);
#746=FACE_OUTER_BOUND('',#929,.T.);
#747=FACE_OUTER_BOUND('',#930,.T.);
#748=FACE_OUTER_BOUND('',#931,.T.);
#749=FACE_OUTER_BOUND('',#932,.T.);
#750=FACE_OUTER_BOUND('',#933,.T.);
#751=FACE_OUTER_BOUND('',#934,.T.);
#752=FACE_OUTER_BOUND('',#935,.T.);
#753=FACE_OUTER_BOUND('',#936,.T.);
#754=FACE_OUTER_BOUND('',#937,.T.);
#755=FACE_OUTER_BOUND('',#940,.T.);
#756=FACE_OUTER_BOUND('',#943,.T.);
#757=FACE_OUTER_BOUND('',#944,.T.);
#758=FACE_OUTER_BOUND('',#945,.T.);
#759=FACE_OUTER_BOUND('',#946,.T.);
#760=FACE_OUTER_BOUND('',#947,.T.);
#761=FACE_OUTER_BOUND('',#948,.T.);
#762=FACE_OUTER_BOUND('',#949,.T.);
#763=FACE_OUTER_BOUND('',#950,.T.);
#764=FACE_OUTER_BOUND('',#951,.T.);
#765=FACE_OUTER_BOUND('',#952,.T.);
#766=FACE_OUTER_BOUND('',#953,.T.);
#767=FACE_OUTER_BOUND('',#954,.T.);
#768=FACE_OUTER_BOUND('',#955,.T.);
#769=FACE_OUTER_BOUND('',#956,.T.);
#770=FACE_OUTER_BOUND('',#957,.T.);
#771=FACE_OUTER_BOUND('',#958,.T.);
#772=FACE_OUTER_BOUND('',#959,.T.);
#773=FACE_OUTER_BOUND('',#962,.T.);
#774=FACE_OUTER_BOUND('',#963,.T.);
#775=FACE_OUTER_BOUND('',#964,.T.);
#776=FACE_OUTER_BOUND('',#965,.T.);
#777=FACE_OUTER_BOUND('',#966,.T.);
#778=FACE_OUTER_BOUND('',#969,.T.);
#779=FACE_OUTER_BOUND('',#970,.T.);
#780=FACE_OUTER_BOUND('',#971,.T.);
#781=FACE_OUTER_BOUND('',#972,.T.);
#782=FACE_OUTER_BOUND('',#973,.T.);
#783=FACE_OUTER_BOUND('',#974,.T.);
#784=FACE_OUTER_BOUND('',#975,.T.);
#785=FACE_OUTER_BOUND('',#976,.T.);
#786=FACE_OUTER_BOUND('',#977,.T.);
#787=FACE_OUTER_BOUND('',#978,.T.);
#788=FACE_OUTER_BOUND('',#979,.T.);
#789=FACE_OUTER_BOUND('',#980,.T.);
#790=FACE_OUTER_BOUND('',#981,.T.);
#791=FACE_OUTER_BOUND('',#982,.T.);
#792=FACE_OUTER_BOUND('',#983,.T.);
#793=FACE_OUTER_BOUND('',#984,.T.);
#794=FACE_OUTER_BOUND('',#985,.T.);
#795=FACE_OUTER_BOUND('',#988,.T.);
#796=FACE_OUTER_BOUND('',#989,.T.);
#797=FACE_OUTER_BOUND('',#990,.T.);
#798=FACE_OUTER_BOUND('',#991,.T.);
#799=FACE_OUTER_BOUND('',#992,.T.);
#800=FACE_OUTER_BOUND('',#995,.T.);
#801=FACE_OUTER_BOUND('',#996,.T.);
#802=FACE_OUTER_BOUND('',#997,.T.);
#803=FACE_OUTER_BOUND('',#998,.T.);
#804=FACE_OUTER_BOUND('',#999,.T.);
#805=FACE_OUTER_BOUND('',#1000,.T.);
#806=FACE_OUTER_BOUND('',#1001,.T.);
#807=FACE_OUTER_BOUND('',#1002,.T.);
#808=FACE_OUTER_BOUND('',#1003,.T.);
#809=FACE_OUTER_BOUND('',#1004,.T.);
#810=FACE_OUTER_BOUND('',#1005,.T.);
#811=FACE_OUTER_BOUND('',#1006,.T.);
#812=FACE_OUTER_BOUND('',#1007,.T.);
#813=FACE_OUTER_BOUND('',#1008,.T.);
#814=FACE_OUTER_BOUND('',#1009,.T.);
#815=FACE_OUTER_BOUND('',#1010,.T.);
#816=FACE_OUTER_BOUND('',#1011,.T.);
#817=FACE_OUTER_BOUND('',#1012,.T.);
#818=FACE_OUTER_BOUND('',#1013,.T.);
#819=FACE_OUTER_BOUND('',#1014,.T.);
#820=FACE_OUTER_BOUND('',#1015,.T.);
#821=FACE_OUTER_BOUND('',#1017,.T.);
#822=FACE_OUTER_BOUND('',#1018,.T.);
#823=FACE_OUTER_BOUND('',#1019,.T.);
#824=FACE_OUTER_BOUND('',#1020,.T.);
#825=FACE_OUTER_BOUND('',#1021,.T.);
#826=FACE_OUTER_BOUND('',#1023,.T.);
#827=FACE_OUTER_BOUND('',#1024,.T.);
#828=FACE_OUTER_BOUND('',#1025,.T.);
#829=FACE_OUTER_BOUND('',#1026,.T.);
#830=FACE_OUTER_BOUND('',#1028,.T.);
#831=FACE_OUTER_BOUND('',#1029,.T.);
#832=FACE_OUTER_BOUND('',#1031,.T.);
#833=FACE_OUTER_BOUND('',#1032,.T.);
#834=FACE_OUTER_BOUND('',#1033,.T.);
#835=FACE_OUTER_BOUND('',#1034,.T.);
#836=FACE_OUTER_BOUND('',#1035,.T.);
#837=FACE_OUTER_BOUND('',#1036,.T.);
#838=FACE_OUTER_BOUND('',#1038,.T.);
#839=FACE_OUTER_BOUND('',#1039,.T.);
#840=FACE_OUTER_BOUND('',#1041,.T.);
#841=FACE_OUTER_BOUND('',#1043,.T.);
#842=FACE_OUTER_BOUND('',#1044,.T.);
#843=FACE_OUTER_BOUND('',#1046,.T.);
#844=FACE_OUTER_BOUND('',#1047,.T.);
#845=FACE_OUTER_BOUND('',#1049,.T.);
#846=FACE_OUTER_BOUND('',#1050,.T.);
#847=FACE_OUTER_BOUND('',#1052,.T.);
#848=FACE_OUTER_BOUND('',#1054,.T.);
#849=FACE_OUTER_BOUND('',#1055,.T.);
#850=FACE_OUTER_BOUND('',#1057,.T.);
#851=FACE_OUTER_BOUND('',#1058,.T.);
#852=FACE_OUTER_BOUND('',#1059,.T.);
#853=FACE_OUTER_BOUND('',#1061,.T.);
#854=FACE_OUTER_BOUND('',#1062,.T.);
#855=FACE_OUTER_BOUND('',#1064,.T.);
#856=FACE_OUTER_BOUND('',#1065,.T.);
#857=FACE_OUTER_BOUND('',#1067,.T.);
#858=FACE_OUTER_BOUND('',#1068,.T.);
#859=FACE_OUTER_BOUND('',#1069,.T.);
#860=FACE_OUTER_BOUND('',#1071,.T.);
#861=FACE_OUTER_BOUND('',#1072,.T.);
#862=FACE_OUTER_BOUND('',#1074,.T.);
#863=FACE_OUTER_BOUND('',#1075,.T.);
#864=FACE_OUTER_BOUND('',#1077,.T.);
#865=EDGE_LOOP('',(#2267,#2268,#2269,#2270));
#866=EDGE_LOOP('',(#2271,#2272,#2273,#2274,#2275,#2276,#2277));
#867=EDGE_LOOP('',(#2278,#2279,#2280,#2281,#2282,#2283,#2284));
#868=EDGE_LOOP('',(#2285,#2286,#2287,#2288,#2289,#2290,#2291,#2292,#2293,
#2294,#2295,#2296,#2297,#2298));
#869=EDGE_LOOP('',(#2299));
#870=EDGE_LOOP('',(#2300));
#871=EDGE_LOOP('',(#2301,#2302,#2303,#2304,#2305,#2306,#2307,#2308,#2309,
#2310,#2311,#2312,#2313,#2314));
#872=EDGE_LOOP('',(#2315));
#873=EDGE_LOOP('',(#2316));
#874=EDGE_LOOP('',(#2317,#2318,#2319,#2320));
#875=EDGE_LOOP('',(#2321,#2322,#2323,#2324));
#876=EDGE_LOOP('',(#2325,#2326,#2327,#2328));
#877=EDGE_LOOP('',(#2329,#2330,#2331,#2332,#2333,#2334,#2335,#2336));
#878=EDGE_LOOP('',(#2337,#2338,#2339,#2340));
#879=EDGE_LOOP('',(#2341,#2342,#2343,#2344));
#880=EDGE_LOOP('',(#2345,#2346,#2347,#2348));
#881=EDGE_LOOP('',(#2349,#2350,#2351,#2352));
#882=EDGE_LOOP('',(#2353,#2354,#2355,#2356));
#883=EDGE_LOOP('',(#2357,#2358,#2359,#2360,#2361,#2362));
#884=EDGE_LOOP('',(#2363,#2364,#2365,#2366));
#885=EDGE_LOOP('',(#2367,#2368,#2369,#2370,#2371,#2372));
#886=EDGE_LOOP('',(#2373,#2374,#2375,#2376));
#887=EDGE_LOOP('',(#2377,#2378,#2379,#2380));
#888=EDGE_LOOP('',(#2381,#2382,#2383,#2384));
#889=EDGE_LOOP('',(#2385,#2386,#2387,#2388,#2389,#2390,#2391));
#890=EDGE_LOOP('',(#2392,#2393,#2394,#2395,#2396,#2397,#2398));
#891=EDGE_LOOP('',(#2399,#2400,#2401,#2402,#2403,#2404,#2405,#2406,#2407,
#2408,#2409,#2410,#2411,#2412));
#892=EDGE_LOOP('',(#2413));
#893=EDGE_LOOP('',(#2414));
#894=EDGE_LOOP('',(#2415,#2416,#2417,#2418,#2419,#2420,#2421,#2422,#2423,
#2424,#2425,#2426,#2427,#2428));
#895=EDGE_LOOP('',(#2429));
#896=EDGE_LOOP('',(#2430));
#897=EDGE_LOOP('',(#2431,#2432,#2433,#2434));
#898=EDGE_LOOP('',(#2435,#2436,#2437,#2438));
#899=EDGE_LOOP('',(#2439,#2440,#2441,#2442));
#900=EDGE_LOOP('',(#2443,#2444,#2445,#2446,#2447,#2448,#2449,#2450));
#901=EDGE_LOOP('',(#2451,#2452,#2453,#2454));
#902=EDGE_LOOP('',(#2455,#2456,#2457,#2458));
#903=EDGE_LOOP('',(#2459,#2460,#2461,#2462));
#904=EDGE_LOOP('',(#2463,#2464,#2465,#2466));
#905=EDGE_LOOP('',(#2467,#2468,#2469,#2470));
#906=EDGE_LOOP('',(#2471,#2472,#2473,#2474,#2475,#2476));
#907=EDGE_LOOP('',(#2477,#2478,#2479,#2480));
#908=EDGE_LOOP('',(#2481,#2482,#2483,#2484,#2485,#2486));
#909=EDGE_LOOP('',(#2487,#2488,#2489,#2490));
#910=EDGE_LOOP('',(#2491,#2492,#2493,#2494));
#911=EDGE_LOOP('',(#2495,#2496,#2497,#2498));
#912=EDGE_LOOP('',(#2499,#2500,#2501,#2502,#2503,#2504,#2505));
#913=EDGE_LOOP('',(#2506,#2507,#2508,#2509,#2510,#2511,#2512));
#914=EDGE_LOOP('',(#2513,#2514,#2515,#2516,#2517,#2518,#2519,#2520,#2521,
#2522,#2523,#2524,#2525,#2526));
#915=EDGE_LOOP('',(#2527));
#916=EDGE_LOOP('',(#2528));
#917=EDGE_LOOP('',(#2529,#2530,#2531,#2532,#2533,#2534,#2535,#2536,#2537,
#2538,#2539,#2540,#2541,#2542));
#918=EDGE_LOOP('',(#2543));
#919=EDGE_LOOP('',(#2544));
#920=EDGE_LOOP('',(#2545,#2546,#2547,#2548));
#921=EDGE_LOOP('',(#2549,#2550,#2551,#2552));
#922=EDGE_LOOP('',(#2553,#2554,#2555,#2556));
#923=EDGE_LOOP('',(#2557,#2558,#2559,#2560,#2561,#2562,#2563,#2564));
#924=EDGE_LOOP('',(#2565,#2566,#2567,#2568));
#925=EDGE_LOOP('',(#2569,#2570,#2571,#2572));
#926=EDGE_LOOP('',(#2573,#2574,#2575,#2576));
#927=EDGE_LOOP('',(#2577,#2578,#2579,#2580));
#928=EDGE_LOOP('',(#2581,#2582,#2583,#2584));
#929=EDGE_LOOP('',(#2585,#2586,#2587,#2588,#2589,#2590));
#930=EDGE_LOOP('',(#2591,#2592,#2593,#2594));
#931=EDGE_LOOP('',(#2595,#2596,#2597,#2598,#2599,#2600));
#932=EDGE_LOOP('',(#2601,#2602,#2603,#2604));
#933=EDGE_LOOP('',(#2605,#2606,#2607,#2608));
#934=EDGE_LOOP('',(#2609,#2610,#2611,#2612));
#935=EDGE_LOOP('',(#2613,#2614,#2615,#2616,#2617,#2618,#2619));
#936=EDGE_LOOP('',(#2620,#2621,#2622,#2623,#2624,#2625,#2626));
#937=EDGE_LOOP('',(#2627,#2628,#2629,#2630,#2631,#2632,#2633,#2634,#2635,
#2636,#2637,#2638,#2639,#2640));
#938=EDGE_LOOP('',(#2641));
#939=EDGE_LOOP('',(#2642));
#940=EDGE_LOOP('',(#2643,#2644,#2645,#2646,#2647,#2648,#2649,#2650,#2651,
#2652,#2653,#2654,#2655,#2656));
#941=EDGE_LOOP('',(#2657));
#942=EDGE_LOOP('',(#2658));
#943=EDGE_LOOP('',(#2659,#2660,#2661,#2662));
#944=EDGE_LOOP('',(#2663,#2664,#2665,#2666));
#945=EDGE_LOOP('',(#2667,#2668,#2669,#2670));
#946=EDGE_LOOP('',(#2671,#2672,#2673,#2674,#2675,#2676,#2677,#2678));
#947=EDGE_LOOP('',(#2679,#2680,#2681,#2682));
#948=EDGE_LOOP('',(#2683,#2684,#2685,#2686));
#949=EDGE_LOOP('',(#2687,#2688,#2689,#2690));
#950=EDGE_LOOP('',(#2691,#2692,#2693,#2694));
#951=EDGE_LOOP('',(#2695,#2696,#2697,#2698));
#952=EDGE_LOOP('',(#2699,#2700,#2701,#2702,#2703,#2704));
#953=EDGE_LOOP('',(#2705,#2706,#2707,#2708));
#954=EDGE_LOOP('',(#2709,#2710,#2711,#2712,#2713,#2714));
#955=EDGE_LOOP('',(#2715,#2716,#2717,#2718));
#956=EDGE_LOOP('',(#2719,#2720,#2721,#2722));
#957=EDGE_LOOP('',(#2723,#2724,#2725,#2726));
#958=EDGE_LOOP('',(#2727,#2728,#2729,#2730));
#959=EDGE_LOOP('',(#2731,#2732,#2733,#2734));
#960=EDGE_LOOP('',(#2735));
#961=EDGE_LOOP('',(#2736));
#962=EDGE_LOOP('',(#2737,#2738,#2739,#2740));
#963=EDGE_LOOP('',(#2741,#2742,#2743,#2744));
#964=EDGE_LOOP('',(#2745,#2746,#2747,#2748));
#965=EDGE_LOOP('',(#2749,#2750,#2751,#2752));
#966=EDGE_LOOP('',(#2753,#2754,#2755,#2756,#2757,#2758,#2759,#2760,#2761,
#2762,#2763,#2764,#2765,#2766));
#967=EDGE_LOOP('',(#2767));
#968=EDGE_LOOP('',(#2768));
#969=EDGE_LOOP('',(#2769));
#970=EDGE_LOOP('',(#2770));
#971=EDGE_LOOP('',(#2771,#2772,#2773,#2774,#2775,#2776,#2777,#2778,#2779,
#2780,#2781,#2782,#2783,#2784));
#972=EDGE_LOOP('',(#2785,#2786,#2787,#2788));
#973=EDGE_LOOP('',(#2789,#2790,#2791,#2792));
#974=EDGE_LOOP('',(#2793,#2794,#2795,#2796));
#975=EDGE_LOOP('',(#2797,#2798,#2799,#2800));
#976=EDGE_LOOP('',(#2801,#2802,#2803,#2804,#2805,#2806,#2807,#2808,#2809));
#977=EDGE_LOOP('',(#2810,#2811,#2812,#2813,#2814,#2815));
#978=EDGE_LOOP('',(#2816,#2817,#2818,#2819,#2820,#2821));
#979=EDGE_LOOP('',(#2822,#2823,#2824,#2825,#2826,#2827));
#980=EDGE_LOOP('',(#2828,#2829,#2830,#2831));
#981=EDGE_LOOP('',(#2832,#2833,#2834,#2835,#2836,#2837,#2838));
#982=EDGE_LOOP('',(#2839,#2840,#2841,#2842));
#983=EDGE_LOOP('',(#2843,#2844,#2845,#2846));
#984=EDGE_LOOP('',(#2847,#2848,#2849,#2850));
#985=EDGE_LOOP('',(#2851,#2852,#2853,#2854));
#986=EDGE_LOOP('',(#2855));
#987=EDGE_LOOP('',(#2856));
#988=EDGE_LOOP('',(#2857,#2858,#2859,#2860));
#989=EDGE_LOOP('',(#2861,#2862,#2863,#2864));
#990=EDGE_LOOP('',(#2865,#2866,#2867,#2868));
#991=EDGE_LOOP('',(#2869,#2870,#2871,#2872));
#992=EDGE_LOOP('',(#2873,#2874,#2875,#2876,#2877,#2878,#2879,#2880,#2881,
#2882,#2883,#2884,#2885,#2886));
#993=EDGE_LOOP('',(#2887));
#994=EDGE_LOOP('',(#2888));
#995=EDGE_LOOP('',(#2889));
#996=EDGE_LOOP('',(#2890));
#997=EDGE_LOOP('',(#2891,#2892,#2893,#2894,#2895,#2896,#2897,#2898,#2899,
#2900,#2901,#2902,#2903,#2904));
#998=EDGE_LOOP('',(#2905,#2906,#2907,#2908));
#999=EDGE_LOOP('',(#2909,#2910,#2911,#2912));
#1000=EDGE_LOOP('',(#2913,#2914,#2915,#2916));
#1001=EDGE_LOOP('',(#2917,#2918,#2919,#2920));
#1002=EDGE_LOOP('',(#2921,#2922,#2923,#2924,#2925,#2926,#2927,#2928,#2929));
#1003=EDGE_LOOP('',(#2930,#2931,#2932,#2933,#2934,#2935));
#1004=EDGE_LOOP('',(#2936,#2937,#2938,#2939,#2940,#2941));
#1005=EDGE_LOOP('',(#2942,#2943,#2944,#2945,#2946,#2947));
#1006=EDGE_LOOP('',(#2948,#2949,#2950,#2951));
#1007=EDGE_LOOP('',(#2952,#2953,#2954,#2955,#2956,#2957,#2958));
#1008=EDGE_LOOP('',(#2959,#2960,#2961,#2962));
#1009=EDGE_LOOP('',(#2963,#2964,#2965,#2966,#2967,#2968));
#1010=EDGE_LOOP('',(#2969));
#1011=EDGE_LOOP('',(#2970));
#1012=EDGE_LOOP('',(#2971,#2972,#2973,#2974,#2975));
#1013=EDGE_LOOP('',(#2976,#2977,#2978,#2979,#2980));
#1014=EDGE_LOOP('',(#2981,#2982,#2983,#2984,#2985));
#1015=EDGE_LOOP('',(#2986));
#1016=EDGE_LOOP('',(#2987));
#1017=EDGE_LOOP('',(#2988,#2989,#2990,#2991,#2992));
#1018=EDGE_LOOP('',(#2993,#2994,#2995,#2996,#2997));
#1019=EDGE_LOOP('',(#2998,#2999,#3000,#3001,#3002));
#1020=EDGE_LOOP('',(#3003,#3004,#3005,#3006,#3007));
#1021=EDGE_LOOP('',(#3008));
#1022=EDGE_LOOP('',(#3009));
#1023=EDGE_LOOP('',(#3010,#3011,#3012,#3013,#3014));
#1024=EDGE_LOOP('',(#3015,#3016,#3017,#3018,#3019));
#1025=EDGE_LOOP('',(#3020,#3021,#3022,#3023,#3024));
#1026=EDGE_LOOP('',(#3025));
#1027=EDGE_LOOP('',(#3026));
#1028=EDGE_LOOP('',(#3027,#3028,#3029,#3030));
#1029=EDGE_LOOP('',(#3031));
#1030=EDGE_LOOP('',(#3032));
#1031=EDGE_LOOP('',(#3033,#3034,#3035,#3036));
#1032=EDGE_LOOP('',(#3037,#3038,#3039,#3040));
#1033=EDGE_LOOP('',(#3041,#3042,#3043,#3044));
#1034=EDGE_LOOP('',(#3045,#3046,#3047,#3048));
#1035=EDGE_LOOP('',(#3049,#3050,#3051,#3052));
#1036=EDGE_LOOP('',(#3053));
#1037=EDGE_LOOP('',(#3054));
#1038=EDGE_LOOP('',(#3055,#3056,#3057,#3058));
#1039=EDGE_LOOP('',(#3059));
#1040=EDGE_LOOP('',(#3060));
#1041=EDGE_LOOP('',(#3061));
#1042=EDGE_LOOP('',(#3062));
#1043=EDGE_LOOP('',(#3063,#3064,#3065,#3066));
#1044=EDGE_LOOP('',(#3067));
#1045=EDGE_LOOP('',(#3068));
#1046=EDGE_LOOP('',(#3069,#3070,#3071,#3072));
#1047=EDGE_LOOP('',(#3073));
#1048=EDGE_LOOP('',(#3074));
#1049=EDGE_LOOP('',(#3075,#3076,#3077,#3078));
#1050=EDGE_LOOP('',(#3079));
#1051=EDGE_LOOP('',(#3080));
#1052=EDGE_LOOP('',(#3081));
#1053=EDGE_LOOP('',(#3082));
#1054=EDGE_LOOP('',(#3083,#3084,#3085,#3086));
#1055=EDGE_LOOP('',(#3087));
#1056=EDGE_LOOP('',(#3088));
#1057=EDGE_LOOP('',(#3089,#3090,#3091,#3092));
#1058=EDGE_LOOP('',(#3093,#3094,#3095,#3096));
#1059=EDGE_LOOP('',(#3097));
#1060=EDGE_LOOP('',(#3098));
#1061=EDGE_LOOP('',(#3099,#3100,#3101,#3102));
#1062=EDGE_LOOP('',(#3103));
#1063=EDGE_LOOP('',(#3104));
#1064=EDGE_LOOP('',(#3105,#3106,#3107,#3108));
#1065=EDGE_LOOP('',(#3109));
#1066=EDGE_LOOP('',(#3110));
#1067=EDGE_LOOP('',(#3111,#3112,#3113,#3114));
#1068=EDGE_LOOP('',(#3115,#3116,#3117,#3118));
#1069=EDGE_LOOP('',(#3119));
#1070=EDGE_LOOP('',(#3120));
#1071=EDGE_LOOP('',(#3121,#3122,#3123,#3124));
#1072=EDGE_LOOP('',(#3125));
#1073=EDGE_LOOP('',(#3126));
#1074=EDGE_LOOP('',(#3127,#3128,#3129,#3130));
#1075=EDGE_LOOP('',(#3131));
#1076=EDGE_LOOP('',(#3132));
#1077=EDGE_LOOP('',(#3133,#3134,#3135,#3136));
#1078=LINE('',#5136,#1311);
#1079=LINE('',#5138,#1312);
#1080=LINE('',#5140,#1313);
#1081=LINE('',#5141,#1314);
#1082=LINE('',#5145,#1315);
#1083=LINE('',#5147,#1316);
#1084=LINE('',#5149,#1317);
#1085=LINE('',#5151,#1318);
#1086=LINE('',#5156,#1319);
#1087=LINE('',#5160,#1320);
#1088=LINE('',#5162,#1321);
#1089=LINE('',#5164,#1322);
#1090=LINE('',#5166,#1323);
#1091=LINE('',#5171,#1324);
#1092=LINE('',#5176,#1325);
#1093=LINE('',#5180,#1326);
#1094=LINE('',#5182,#1327);
#1095=LINE('',#5186,#1328);
#1096=LINE('',#5190,#1329);
#1097=LINE('',#5199,#1330);
#1098=LINE('',#5203,#1331);
#1099=LINE('',#5205,#1332);
#1100=LINE('',#5209,#1333);
#1101=LINE('',#5213,#1334);
#1102=LINE('',#5221,#1335);
#1103=LINE('',#5223,#1336);
#1104=LINE('',#5226,#1337);
#1105=LINE('',#5264,#1338);
#1106=LINE('',#5265,#1339);
#1107=LINE('',#5267,#1340);
#1108=LINE('',#5268,#1341);
#1109=LINE('',#5270,#1342);
#1110=LINE('',#5271,#1343);
#1111=LINE('',#5273,#1344);
#1112=LINE('',#5274,#1345);
#1113=LINE('',#5285,#1346);
#1114=LINE('',#5287,#1347);
#1115=LINE('',#5289,#1348);
#1116=LINE('',#5290,#1349);
#1117=LINE('',#5294,#1350);
#1118=LINE('',#5296,#1351);
#1119=LINE('',#5298,#1352);
#1120=LINE('',#5300,#1353);
#1121=LINE('',#5305,#1354);
#1122=LINE('',#5309,#1355);
#1123=LINE('',#5311,#1356);
#1124=LINE('',#5313,#1357);
#1125=LINE('',#5315,#1358);
#1126=LINE('',#5320,#1359);
#1127=LINE('',#5325,#1360);
#1128=LINE('',#5329,#1361);
#1129=LINE('',#5331,#1362);
#1130=LINE('',#5335,#1363);
#1131=LINE('',#5339,#1364);
#1132=LINE('',#5348,#1365);
#1133=LINE('',#5352,#1366);
#1134=LINE('',#5354,#1367);
#1135=LINE('',#5358,#1368);
#1136=LINE('',#5362,#1369);
#1137=LINE('',#5370,#1370);
#1138=LINE('',#5372,#1371);
#1139=LINE('',#5375,#1372);
#1140=LINE('',#5413,#1373);
#1141=LINE('',#5414,#1374);
#1142=LINE('',#5416,#1375);
#1143=LINE('',#5417,#1376);
#1144=LINE('',#5419,#1377);
#1145=LINE('',#5420,#1378);
#1146=LINE('',#5422,#1379);
#1147=LINE('',#5423,#1380);
#1148=LINE('',#5434,#1381);
#1149=LINE('',#5436,#1382);
#1150=LINE('',#5438,#1383);
#1151=LINE('',#5439,#1384);
#1152=LINE('',#5443,#1385);
#1153=LINE('',#5445,#1386);
#1154=LINE('',#5451,#1387);
#1155=LINE('',#5453,#1388);
#1156=LINE('',#5454,#1389);
#1157=LINE('',#5458,#1390);
#1158=LINE('',#5460,#1391);
#1159=LINE('',#5466,#1392);
#1160=LINE('',#5468,#1393);
#1161=LINE('',#5469,#1394);
#1162=LINE('',#5474,#1395);
#1163=LINE('',#5478,#1396);
#1164=LINE('',#5480,#1397);
#1165=LINE('',#5484,#1398);
#1166=LINE('',#5488,#1399);
#1167=LINE('',#5497,#1400);
#1168=LINE('',#5502,#1401);
#1169=LINE('',#5506,#1402);
#1170=LINE('',#5508,#1403);
#1171=LINE('',#5512,#1404);
#1172=LINE('',#5519,#1405);
#1173=LINE('',#5521,#1406);
#1174=LINE('',#5542,#1407);
#1175=LINE('',#5562,#1408);
#1176=LINE('',#5563,#1409);
#1177=LINE('',#5565,#1410);
#1178=LINE('',#5566,#1411);
#1179=LINE('',#5568,#1412);
#1180=LINE('',#5569,#1413);
#1181=LINE('',#5571,#1414);
#1182=LINE('',#5572,#1415);
#1183=LINE('',#5583,#1416);
#1184=LINE('',#5585,#1417);
#1185=LINE('',#5587,#1418);
#1186=LINE('',#5588,#1419);
#1187=LINE('',#5592,#1420);
#1188=LINE('',#5594,#1421);
#1189=LINE('',#5600,#1422);
#1190=LINE('',#5602,#1423);
#1191=LINE('',#5603,#1424);
#1192=LINE('',#5607,#1425);
#1193=LINE('',#5609,#1426);
#1194=LINE('',#5615,#1427);
#1195=LINE('',#5617,#1428);
#1196=LINE('',#5618,#1429);
#1197=LINE('',#5623,#1430);
#1198=LINE('',#5627,#1431);
#1199=LINE('',#5629,#1432);
#1200=LINE('',#5633,#1433);
#1201=LINE('',#5637,#1434);
#1202=LINE('',#5646,#1435);
#1203=LINE('',#5651,#1436);
#1204=LINE('',#5655,#1437);
#1205=LINE('',#5657,#1438);
#1206=LINE('',#5661,#1439);
#1207=LINE('',#5668,#1440);
#1208=LINE('',#5670,#1441);
#1209=LINE('',#5691,#1442);
#1210=LINE('',#5711,#1443);
#1211=LINE('',#5712,#1444);
#1212=LINE('',#5714,#1445);
#1213=LINE('',#5715,#1446);
#1214=LINE('',#5717,#1447);
#1215=LINE('',#5718,#1448);
#1216=LINE('',#5720,#1449);
#1217=LINE('',#5721,#1450);
#1218=LINE('',#5733,#1451);
#1219=LINE('',#5735,#1452);
#1220=LINE('',#5737,#1453);
#1221=LINE('',#5738,#1454);
#1222=LINE('',#5742,#1455);
#1223=LINE('',#5744,#1456);
#1224=LINE('',#5746,#1457);
#1225=LINE('',#5747,#1458);
#1226=LINE('',#5751,#1459);
#1227=LINE('',#5753,#1460);
#1228=LINE('',#5755,#1461);
#1229=LINE('',#5756,#1462);
#1230=LINE('',#5764,#1463);
#1231=LINE('',#5766,#1464);
#1232=LINE('',#5768,#1465);
#1233=LINE('',#5769,#1466);
#1234=LINE('',#5774,#1467);
#1235=LINE('',#5779,#1468);
#1236=LINE('',#5781,#1469);
#1237=LINE('',#5783,#1470);
#1238=LINE('',#5784,#1471);
#1239=LINE('',#5789,#1472);
#1240=LINE('',#5794,#1473);
#1241=LINE('',#5817,#1474);
#1242=LINE('',#5827,#1475);
#1243=LINE('',#5830,#1476);
#1244=LINE('',#5832,#1477);
#1245=LINE('',#5837,#1478);
#1246=LINE('',#5840,#1479);
#1247=LINE('',#5854,#1480);
#1248=LINE('',#5866,#1481);
#1249=LINE('',#5869,#1482);
#1250=LINE('',#5875,#1483);
#1251=LINE('',#5877,#1484);
#1252=LINE('',#5879,#1485);
#1253=LINE('',#5880,#1486);
#1254=LINE('',#5884,#1487);
#1255=LINE('',#5886,#1488);
#1256=LINE('',#5888,#1489);
#1257=LINE('',#5889,#1490);
#1258=LINE('',#5893,#1491);
#1259=LINE('',#5895,#1492);
#1260=LINE('',#5897,#1493);
#1261=LINE('',#5898,#1494);
#1262=LINE('',#5906,#1495);
#1263=LINE('',#5908,#1496);
#1264=LINE('',#5910,#1497);
#1265=LINE('',#5911,#1498);
#1266=LINE('',#5916,#1499);
#1267=LINE('',#5921,#1500);
#1268=LINE('',#5923,#1501);
#1269=LINE('',#5925,#1502);
#1270=LINE('',#5926,#1503);
#1271=LINE('',#5931,#1504);
#1272=LINE('',#5936,#1505);
#1273=LINE('',#5955,#1506);
#1274=LINE('',#5969,#1507);
#1275=LINE('',#5974,#1508);
#1276=LINE('',#5976,#1509);
#1277=LINE('',#5979,#1510);
#1278=LINE('',#5982,#1511);
#1279=LINE('',#5996,#1512);
#1280=LINE('',#6008,#1513);
#1281=LINE('',#6011,#1514);
#1282=LINE('',#6019,#1515);
#1283=LINE('',#6051,#1516);
#1284=LINE('',#6059,#1517);
#1285=LINE('',#6065,#1518);
#1286=LINE('',#6070,#1519);
#1287=LINE('',#6076,#1520);
#1288=LINE('',#6085,#1521);
#1289=LINE('',#6090,#1522);
#1290=LINE('',#6094,#1523);
#1291=LINE('',#6102,#1524);
#1292=LINE('',#6109,#1525);
#1293=LINE('',#6113,#1526);
#1294=LINE('',#6117,#1527);
#1295=LINE('',#6120,#1528);
#1296=LINE('',#6125,#1529);
#1297=LINE('',#6132,#1530);
#1298=LINE('',#6140,#1531);
#1299=LINE('',#6147,#1532);
#1300=LINE('',#6154,#1533);
#1301=LINE('',#6164,#1534);
#1302=LINE('',#6172,#1535);
#1303=LINE('',#6175,#1536);
#1304=LINE('',#6181,#1537);
#1305=LINE('',#6191,#1538);
#1306=LINE('',#6198,#1539);
#1307=LINE('',#6202,#1540);
#1308=LINE('',#6207,#1541);
#1309=LINE('',#6216,#1542);
#1310=LINE('',#6222,#1543);
#1311=VECTOR('',#3986,1.);
#1312=VECTOR('',#3987,1.);
#1313=VECTOR('',#3988,1.);
#1314=VECTOR('',#3989,1.);
#1315=VECTOR('',#3992,1.);
#1316=VECTOR('',#3993,1.);
#1317=VECTOR('',#3994,1.);
#1318=VECTOR('',#3995,1.);
#1319=VECTOR('',#4000,1.);
#1320=VECTOR('',#4003,1.);
#1321=VECTOR('',#4004,1.);
#1322=VECTOR('',#4005,1.);
#1323=VECTOR('',#4006,1.);
#1324=VECTOR('',#4011,1.);
#1325=VECTOR('',#4016,1.);
#1326=VECTOR('',#4019,1.);
#1327=VECTOR('',#4022,1.);
#1328=VECTOR('',#4025,1.);
#1329=VECTOR('',#4028,1.);
#1330=VECTOR('',#4037,1.);
#1331=VECTOR('',#4040,1.);
#1332=VECTOR('',#4043,1.);
#1333=VECTOR('',#4046,1.);
#1334=VECTOR('',#4049,1.);
#1335=VECTOR('',#4060,0.004225);
#1336=VECTOR('',#4063,0.004225);
#1337=VECTOR('',#4068,0.0075);
#1338=VECTOR('',#4071,1.);
#1339=VECTOR('',#4072,1.);
#1340=VECTOR('',#4075,1.);
#1341=VECTOR('',#4076,1.);
#1342=VECTOR('',#4079,1.);
#1343=VECTOR('',#4080,1.);
#1344=VECTOR('',#4083,1.);
#1345=VECTOR('',#4084,1.);
#1346=VECTOR('',#4101,1.);
#1347=VECTOR('',#4102,1.);
#1348=VECTOR('',#4103,1.);
#1349=VECTOR('',#4104,1.);
#1350=VECTOR('',#4107,1.);
#1351=VECTOR('',#4108,1.);
#1352=VECTOR('',#4109,1.);
#1353=VECTOR('',#4110,1.);
#1354=VECTOR('',#4115,1.);
#1355=VECTOR('',#4118,1.);
#1356=VECTOR('',#4119,1.);
#1357=VECTOR('',#4120,1.);
#1358=VECTOR('',#4121,1.);
#1359=VECTOR('',#4126,1.);
#1360=VECTOR('',#4131,1.);
#1361=VECTOR('',#4134,1.);
#1362=VECTOR('',#4137,1.);
#1363=VECTOR('',#4140,1.);
#1364=VECTOR('',#4143,1.);
#1365=VECTOR('',#4152,1.);
#1366=VECTOR('',#4155,1.);
#1367=VECTOR('',#4158,1.);
#1368=VECTOR('',#4161,1.);
#1369=VECTOR('',#4164,1.);
#1370=VECTOR('',#4175,0.004225);
#1371=VECTOR('',#4178,0.004225);
#1372=VECTOR('',#4183,0.0075);
#1373=VECTOR('',#4186,1.);
#1374=VECTOR('',#4187,1.);
#1375=VECTOR('',#4190,1.);
#1376=VECTOR('',#4191,1.);
#1377=VECTOR('',#4194,1.);
#1378=VECTOR('',#4195,1.);
#1379=VECTOR('',#4198,1.);
#1380=VECTOR('',#4199,1.);
#1381=VECTOR('',#4216,1.);
#1382=VECTOR('',#4217,1.);
#1383=VECTOR('',#4218,1.);
#1384=VECTOR('',#4219,1.);
#1385=VECTOR('',#4222,1.);
#1386=VECTOR('',#4223,1.);
#1387=VECTOR('',#4228,1.);
#1388=VECTOR('',#4229,1.);
#1389=VECTOR('',#4230,1.);
#1390=VECTOR('',#4233,1.);
#1391=VECTOR('',#4234,1.);
#1392=VECTOR('',#4239,1.);
#1393=VECTOR('',#4240,1.);
#1394=VECTOR('',#4241,1.);
#1395=VECTOR('',#4246,1.);
#1396=VECTOR('',#4249,1.);
#1397=VECTOR('',#4252,1.);
#1398=VECTOR('',#4255,1.);
#1399=VECTOR('',#4258,1.);
#1400=VECTOR('',#4267,1.);
#1401=VECTOR('',#4272,1.);
#1402=VECTOR('',#4275,1.);
#1403=VECTOR('',#4278,1.);
#1404=VECTOR('',#4281,1.);
#1405=VECTOR('',#4290,0.004225);
#1406=VECTOR('',#4293,0.004225);
#1407=VECTOR('',#4298,0.0075);
#1408=VECTOR('',#4301,1.);
#1409=VECTOR('',#4302,1.);
#1410=VECTOR('',#4305,1.);
#1411=VECTOR('',#4306,1.);
#1412=VECTOR('',#4309,1.);
#1413=VECTOR('',#4310,1.);
#1414=VECTOR('',#4313,1.);
#1415=VECTOR('',#4314,1.);
#1416=VECTOR('',#4331,1.);
#1417=VECTOR('',#4332,1.);
#1418=VECTOR('',#4333,1.);
#1419=VECTOR('',#4334,1.);
#1420=VECTOR('',#4337,1.);
#1421=VECTOR('',#4338,1.);
#1422=VECTOR('',#4343,1.);
#1423=VECTOR('',#4344,1.);
#1424=VECTOR('',#4345,1.);
#1425=VECTOR('',#4348,1.);
#1426=VECTOR('',#4349,1.);
#1427=VECTOR('',#4354,1.);
#1428=VECTOR('',#4355,1.);
#1429=VECTOR('',#4356,1.);
#1430=VECTOR('',#4361,1.);
#1431=VECTOR('',#4364,1.);
#1432=VECTOR('',#4367,1.);
#1433=VECTOR('',#4370,1.);
#1434=VECTOR('',#4373,1.);
#1435=VECTOR('',#4382,1.);
#1436=VECTOR('',#4387,1.);
#1437=VECTOR('',#4390,1.);
#1438=VECTOR('',#4393,1.);
#1439=VECTOR('',#4396,1.);
#1440=VECTOR('',#4405,0.004225);
#1441=VECTOR('',#4408,0.004225);
#1442=VECTOR('',#4413,0.0075);
#1443=VECTOR('',#4416,1.);
#1444=VECTOR('',#4417,1.);
#1445=VECTOR('',#4420,1.);
#1446=VECTOR('',#4421,1.);
#1447=VECTOR('',#4424,1.);
#1448=VECTOR('',#4425,1.);
#1449=VECTOR('',#4428,1.);
#1450=VECTOR('',#4429,1.);
#1451=VECTOR('',#4448,1.);
#1452=VECTOR('',#4449,1.);
#1453=VECTOR('',#4450,1.);
#1454=VECTOR('',#4451,1.);
#1455=VECTOR('',#4454,1.);
#1456=VECTOR('',#4455,1.);
#1457=VECTOR('',#4456,1.);
#1458=VECTOR('',#4457,1.);
#1459=VECTOR('',#4460,1.);
#1460=VECTOR('',#4461,1.);
#1461=VECTOR('',#4462,1.);
#1462=VECTOR('',#4463,1.);
#1463=VECTOR('',#4470,1.);
#1464=VECTOR('',#4471,1.);
#1465=VECTOR('',#4472,1.);
#1466=VECTOR('',#4473,1.);
#1467=VECTOR('',#4478,0.004225);
#1468=VECTOR('',#4483,1.);
#1469=VECTOR('',#4484,1.);
#1470=VECTOR('',#4485,1.);
#1471=VECTOR('',#4486,1.);
#1472=VECTOR('',#4491,0.004225);
#1473=VECTOR('',#4496,1.);
#1474=VECTOR('',#4531,1.);
#1475=VECTOR('',#4546,1.);
#1476=VECTOR('',#4549,1.);
#1477=VECTOR('',#4550,1.);
#1478=VECTOR('',#4555,1.);
#1479=VECTOR('',#4558,0.007625);
#1480=VECTOR('',#4561,0.007625);
#1481=VECTOR('',#4564,1.);
#1482=VECTOR('',#4569,1.);
#1483=VECTOR('',#4576,1.);
#1484=VECTOR('',#4577,1.);
#1485=VECTOR('',#4578,1.);
#1486=VECTOR('',#4579,1.);
#1487=VECTOR('',#4582,1.);
#1488=VECTOR('',#4583,1.);
#1489=VECTOR('',#4584,1.);
#1490=VECTOR('',#4585,1.);
#1491=VECTOR('',#4588,1.);
#1492=VECTOR('',#4589,1.);
#1493=VECTOR('',#4590,1.);
#1494=VECTOR('',#4591,1.);
#1495=VECTOR('',#4598,1.);
#1496=VECTOR('',#4599,1.);
#1497=VECTOR('',#4600,1.);
#1498=VECTOR('',#4601,1.);
#1499=VECTOR('',#4606,0.004225);
#1500=VECTOR('',#4611,1.);
#1501=VECTOR('',#4612,1.);
#1502=VECTOR('',#4613,1.);
#1503=VECTOR('',#4614,1.);
#1504=VECTOR('',#4619,0.004225);
#1505=VECTOR('',#4624,1.);
#1506=VECTOR('',#4651,1.);
#1507=VECTOR('',#4674,1.);
#1508=VECTOR('',#4679,1.);
#1509=VECTOR('',#4680,1.);
#1510=VECTOR('',#4683,1.);
#1511=VECTOR('',#4686,0.007625);
#1512=VECTOR('',#4689,0.007625);
#1513=VECTOR('',#4692,1.);
#1514=VECTOR('',#4697,1.);
#1515=VECTOR('',#4706,0.004);
#1516=VECTOR('',#4757,0.0066);
#1517=VECTOR('',#4768,0.0065);
#1518=VECTOR('',#4775,0.0074);
#1519=VECTOR('',#4782,0.0075);
#1520=VECTOR('',#4787,0.0066);
#1521=VECTOR('',#4800,0.0065);
#1522=VECTOR('',#4805,0.0074);
#1523=VECTOR('',#4810,0.0075);
#1524=VECTOR('',#4821,0.00700000010430813);
#1525=VECTOR('',#4830,0.0063);
#1526=VECTOR('',#4835,0.0061);
#1527=VECTOR('',#4840,0.0059);
#1528=VECTOR('',#4843,0.0061);
#1529=VECTOR('',#4850,0.0063);
#1530=VECTOR('',#4859,0.00700000010430813);
#1531=VECTOR('',#4870,0.00715);
#1532=VECTOR('',#4879,0.0075);
#1533=VECTOR('',#4888,0.00715);
#1534=VECTOR('',#4901,0.0065);
#1535=VECTOR('',#4912,0.0043);
#1536=VECTOR('',#4915,0.00405);
#1537=VECTOR('',#4924,0.0046499998960644);
#1538=VECTOR('',#4937,0.0065);
#1539=VECTOR('',#4946,0.0043);
#1540=VECTOR('',#4951,0.00405);
#1541=VECTOR('',#4958,0.0046499998960644);
#1542=VECTOR('',#4969,0.007);
#1543=VECTOR('',#4978,0.0043);
#1544=VERTEX_POINT('',#5134);
#1545=VERTEX_POINT('',#5135);
#1546=VERTEX_POINT('',#5137);
#1547=VERTEX_POINT('',#5139);
#1548=VERTEX_POINT('',#5143);
#1549=VERTEX_POINT('',#5144);
#1550=VERTEX_POINT('',#5146);
#1551=VERTEX_POINT('',#5148);
#1552=VERTEX_POINT('',#5150);
#1553=VERTEX_POINT('',#5152);
#1554=VERTEX_POINT('',#5154);
#1555=VERTEX_POINT('',#5158);
#1556=VERTEX_POINT('',#5159);
#1557=VERTEX_POINT('',#5161);
#1558=VERTEX_POINT('',#5163);
#1559=VERTEX_POINT('',#5165);
#1560=VERTEX_POINT('',#5167);
#1561=VERTEX_POINT('',#5169);
#1562=VERTEX_POINT('',#5173);
#1563=VERTEX_POINT('',#5175);
#1564=VERTEX_POINT('',#5177);
#1565=VERTEX_POINT('',#5179);
#1566=VERTEX_POINT('',#5183);
#1567=VERTEX_POINT('',#5185);
#1568=VERTEX_POINT('',#5187);
#1569=VERTEX_POINT('',#5189);
#1570=VERTEX_POINT('',#5192);
#1571=VERTEX_POINT('',#5194);
#1572=VERTEX_POINT('',#5197);
#1573=VERTEX_POINT('',#5198);
#1574=VERTEX_POINT('',#5200);
#1575=VERTEX_POINT('',#5202);
#1576=VERTEX_POINT('',#5206);
#1577=VERTEX_POINT('',#5208);
#1578=VERTEX_POINT('',#5210);
#1579=VERTEX_POINT('',#5212);
#1580=VERTEX_POINT('',#5216);
#1581=VERTEX_POINT('',#5218);
#1582=VERTEX_POINT('',#5283);
#1583=VERTEX_POINT('',#5284);
#1584=VERTEX_POINT('',#5286);
#1585=VERTEX_POINT('',#5288);
#1586=VERTEX_POINT('',#5292);
#1587=VERTEX_POINT('',#5293);
#1588=VERTEX_POINT('',#5295);
#1589=VERTEX_POINT('',#5297);
#1590=VERTEX_POINT('',#5299);
#1591=VERTEX_POINT('',#5301);
#1592=VERTEX_POINT('',#5303);
#1593=VERTEX_POINT('',#5307);
#1594=VERTEX_POINT('',#5308);
#1595=VERTEX_POINT('',#5310);
#1596=VERTEX_POINT('',#5312);
#1597=VERTEX_POINT('',#5314);
#1598=VERTEX_POINT('',#5316);
#1599=VERTEX_POINT('',#5318);
#1600=VERTEX_POINT('',#5322);
#1601=VERTEX_POINT('',#5324);
#1602=VERTEX_POINT('',#5326);
#1603=VERTEX_POINT('',#5328);
#1604=VERTEX_POINT('',#5332);
#1605=VERTEX_POINT('',#5334);
#1606=VERTEX_POINT('',#5336);
#1607=VERTEX_POINT('',#5338);
#1608=VERTEX_POINT('',#5341);
#1609=VERTEX_POINT('',#5343);
#1610=VERTEX_POINT('',#5346);
#1611=VERTEX_POINT('',#5347);
#1612=VERTEX_POINT('',#5349);
#1613=VERTEX_POINT('',#5351);
#1614=VERTEX_POINT('',#5355);
#1615=VERTEX_POINT('',#5357);
#1616=VERTEX_POINT('',#5359);
#1617=VERTEX_POINT('',#5361);
#1618=VERTEX_POINT('',#5365);
#1619=VERTEX_POINT('',#5367);
#1620=VERTEX_POINT('',#5432);
#1621=VERTEX_POINT('',#5433);
#1622=VERTEX_POINT('',#5435);
#1623=VERTEX_POINT('',#5437);
#1624=VERTEX_POINT('',#5441);
#1625=VERTEX_POINT('',#5442);
#1626=VERTEX_POINT('',#5444);
#1627=VERTEX_POINT('',#5446);
#1628=VERTEX_POINT('',#5448);
#1629=VERTEX_POINT('',#5450);
#1630=VERTEX_POINT('',#5452);
#1631=VERTEX_POINT('',#5456);
#1632=VERTEX_POINT('',#5457);
#1633=VERTEX_POINT('',#5459);
#1634=VERTEX_POINT('',#5461);
#1635=VERTEX_POINT('',#5463);
#1636=VERTEX_POINT('',#5465);
#1637=VERTEX_POINT('',#5467);
#1638=VERTEX_POINT('',#5471);
#1639=VERTEX_POINT('',#5473);
#1640=VERTEX_POINT('',#5475);
#1641=VERTEX_POINT('',#5477);
#1642=VERTEX_POINT('',#5481);
#1643=VERTEX_POINT('',#5483);
#1644=VERTEX_POINT('',#5485);
#1645=VERTEX_POINT('',#5487);
#1646=VERTEX_POINT('',#5490);
#1647=VERTEX_POINT('',#5492);
#1648=VERTEX_POINT('',#5495);
#1649=VERTEX_POINT('',#5496);
#1650=VERTEX_POINT('',#5499);
#1651=VERTEX_POINT('',#5501);
#1652=VERTEX_POINT('',#5503);
#1653=VERTEX_POINT('',#5505);
#1654=VERTEX_POINT('',#5509);
#1655=VERTEX_POINT('',#5511);
#1656=VERTEX_POINT('',#5514);
#1657=VERTEX_POINT('',#5516);
#1658=VERTEX_POINT('',#5581);
#1659=VERTEX_POINT('',#5582);
#1660=VERTEX_POINT('',#5584);
#1661=VERTEX_POINT('',#5586);
#1662=VERTEX_POINT('',#5590);
#1663=VERTEX_POINT('',#5591);
#1664=VERTEX_POINT('',#5593);
#1665=VERTEX_POINT('',#5595);
#1666=VERTEX_POINT('',#5597);
#1667=VERTEX_POINT('',#5599);
#1668=VERTEX_POINT('',#5601);
#1669=VERTEX_POINT('',#5605);
#1670=VERTEX_POINT('',#5606);
#1671=VERTEX_POINT('',#5608);
#1672=VERTEX_POINT('',#5610);
#1673=VERTEX_POINT('',#5612);
#1674=VERTEX_POINT('',#5614);
#1675=VERTEX_POINT('',#5616);
#1676=VERTEX_POINT('',#5620);
#1677=VERTEX_POINT('',#5622);
#1678=VERTEX_POINT('',#5624);
#1679=VERTEX_POINT('',#5626);
#1680=VERTEX_POINT('',#5630);
#1681=VERTEX_POINT('',#5632);
#1682=VERTEX_POINT('',#5634);
#1683=VERTEX_POINT('',#5636);
#1684=VERTEX_POINT('',#5639);
#1685=VERTEX_POINT('',#5641);
#1686=VERTEX_POINT('',#5644);
#1687=VERTEX_POINT('',#5645);
#1688=VERTEX_POINT('',#5648);
#1689=VERTEX_POINT('',#5650);
#1690=VERTEX_POINT('',#5652);
#1691=VERTEX_POINT('',#5654);
#1692=VERTEX_POINT('',#5658);
#1693=VERTEX_POINT('',#5660);
#1694=VERTEX_POINT('',#5663);
#1695=VERTEX_POINT('',#5665);
#1696=VERTEX_POINT('',#5731);
#1697=VERTEX_POINT('',#5732);
#1698=VERTEX_POINT('',#5734);
#1699=VERTEX_POINT('',#5736);
#1700=VERTEX_POINT('',#5740);
#1701=VERTEX_POINT('',#5741);
#1702=VERTEX_POINT('',#5743);
#1703=VERTEX_POINT('',#5745);
#1704=VERTEX_POINT('',#5749);
#1705=VERTEX_POINT('',#5750);
#1706=VERTEX_POINT('',#5752);
#1707=VERTEX_POINT('',#5754);
#1708=VERTEX_POINT('',#5757);
#1709=VERTEX_POINT('',#5759);
#1710=VERTEX_POINT('',#5762);
#1711=VERTEX_POINT('',#5763);
#1712=VERTEX_POINT('',#5765);
#1713=VERTEX_POINT('',#5767);
#1714=VERTEX_POINT('',#5771);
#1715=VERTEX_POINT('',#5773);
#1716=VERTEX_POINT('',#5777);
#1717=VERTEX_POINT('',#5778);
#1718=VERTEX_POINT('',#5780);
#1719=VERTEX_POINT('',#5782);
#1720=VERTEX_POINT('',#5786);
#1721=VERTEX_POINT('',#5788);
#1722=VERTEX_POINT('',#5792);
#1723=VERTEX_POINT('',#5793);
#1724=VERTEX_POINT('',#5795);
#1725=VERTEX_POINT('',#5802);
#1726=VERTEX_POINT('',#5812);
#1727=VERTEX_POINT('',#5814);
#1728=VERTEX_POINT('',#5816);
#1729=VERTEX_POINT('',#5818);
#1730=VERTEX_POINT('',#5826);
#1731=VERTEX_POINT('',#5828);
#1732=VERTEX_POINT('',#5831);
#1733=VERTEX_POINT('',#5833);
#1734=VERTEX_POINT('',#5835);
#1735=VERTEX_POINT('',#5839);
#1736=VERTEX_POINT('',#5873);
#1737=VERTEX_POINT('',#5874);
#1738=VERTEX_POINT('',#5876);
#1739=VERTEX_POINT('',#5878);
#1740=VERTEX_POINT('',#5882);
#1741=VERTEX_POINT('',#5883);
#1742=VERTEX_POINT('',#5885);
#1743=VERTEX_POINT('',#5887);
#1744=VERTEX_POINT('',#5891);
#1745=VERTEX_POINT('',#5892);
#1746=VERTEX_POINT('',#5894);
#1747=VERTEX_POINT('',#5896);
#1748=VERTEX_POINT('',#5899);
#1749=VERTEX_POINT('',#5901);
#1750=VERTEX_POINT('',#5904);
#1751=VERTEX_POINT('',#5905);
#1752=VERTEX_POINT('',#5907);
#1753=VERTEX_POINT('',#5909);
#1754=VERTEX_POINT('',#5913);
#1755=VERTEX_POINT('',#5915);
#1756=VERTEX_POINT('',#5919);
#1757=VERTEX_POINT('',#5920);
#1758=VERTEX_POINT('',#5922);
#1759=VERTEX_POINT('',#5924);
#1760=VERTEX_POINT('',#5928);
#1761=VERTEX_POINT('',#5930);
#1762=VERTEX_POINT('',#5934);
#1763=VERTEX_POINT('',#5935);
#1764=VERTEX_POINT('',#5937);
#1765=VERTEX_POINT('',#5944);
#1766=VERTEX_POINT('',#5950);
#1767=VERTEX_POINT('',#5952);
#1768=VERTEX_POINT('',#5954);
#1769=VERTEX_POINT('',#5956);
#1770=VERTEX_POINT('',#5968);
#1771=VERTEX_POINT('',#5970);
#1772=VERTEX_POINT('',#5972);
#1773=VERTEX_POINT('',#5975);
#1774=VERTEX_POINT('',#5977);
#1775=VERTEX_POINT('',#5981);
#1776=VERTEX_POINT('',#6015);
#1777=VERTEX_POINT('',#6016);
#1778=VERTEX_POINT('',#6018);
#1779=VERTEX_POINT('',#6020);
#1780=VERTEX_POINT('',#6025);
#1781=VERTEX_POINT('',#6028);
#1782=VERTEX_POINT('',#6047);
#1783=VERTEX_POINT('',#6048);
#1784=VERTEX_POINT('',#6050);
#1785=VERTEX_POINT('',#6055);
#1786=VERTEX_POINT('',#6058);
#1787=VERTEX_POINT('',#6062);
#1788=VERTEX_POINT('',#6063);
#1789=VERTEX_POINT('',#6068);
#1790=VERTEX_POINT('',#6072);
#1791=VERTEX_POINT('',#6073);
#1792=VERTEX_POINT('',#6075);
#1793=VERTEX_POINT('',#6080);
#1794=VERTEX_POINT('',#6083);
#1795=VERTEX_POINT('',#6087);
#1796=VERTEX_POINT('',#6088);
#1797=VERTEX_POINT('',#6093);
#1798=VERTEX_POINT('',#6097);
#1799=VERTEX_POINT('',#6100);
#1800=VERTEX_POINT('',#6104);
#1801=VERTEX_POINT('',#6107);
#1802=VERTEX_POINT('',#6111);
#1803=VERTEX_POINT('',#6115);
#1804=VERTEX_POINT('',#6119);
#1805=VERTEX_POINT('',#6123);
#1806=VERTEX_POINT('',#6127);
#1807=VERTEX_POINT('',#6130);
#1808=VERTEX_POINT('',#6135);
#1809=VERTEX_POINT('',#6138);
#1810=VERTEX_POINT('',#6142);
#1811=VERTEX_POINT('',#6145);
#1812=VERTEX_POINT('',#6149);
#1813=VERTEX_POINT('',#6152);
#1814=VERTEX_POINT('',#6158);
#1815=VERTEX_POINT('',#6160);
#1816=VERTEX_POINT('',#6163);
#1817=VERTEX_POINT('',#6167);
#1818=VERTEX_POINT('',#6170);
#1819=VERTEX_POINT('',#6174);
#1820=VERTEX_POINT('',#6178);
#1821=VERTEX_POINT('',#6184);
#1822=VERTEX_POINT('',#6186);
#1823=VERTEX_POINT('',#6189);
#1824=VERTEX_POINT('',#6193);
#1825=VERTEX_POINT('',#6196);
#1826=VERTEX_POINT('',#6200);
#1827=VERTEX_POINT('',#6204);
#1828=VERTEX_POINT('',#6210);
#1829=VERTEX_POINT('',#6212);
#1830=VERTEX_POINT('',#6215);
#1831=VERTEX_POINT('',#6219);
#1832=EDGE_CURVE('',#1544,#1545,#1078,.T.);
#1833=EDGE_CURVE('',#1546,#1544,#1079,.F.);
#1834=EDGE_CURVE('',#1546,#1547,#1080,.T.);
#1835=EDGE_CURVE('',#1545,#1547,#1081,.T.);
#1836=EDGE_CURVE('',#1548,#1549,#1082,.T.);
#1837=EDGE_CURVE('',#1549,#1550,#1083,.T.);
#1838=EDGE_CURVE('',#1551,#1550,#1084,.T.);
#1839=EDGE_CURVE('',#1552,#1551,#1085,.F.);
#1840=EDGE_CURVE('',#1553,#1552,#506,.T.);
#1841=EDGE_CURVE('',#1554,#1553,#507,.T.);
#1842=EDGE_CURVE('',#1548,#1554,#1086,.F.);
#1843=EDGE_CURVE('',#1555,#1556,#1087,.T.);
#1844=EDGE_CURVE('',#1557,#1556,#1088,.T.);
#1845=EDGE_CURVE('',#1558,#1557,#1089,.T.);
#1846=EDGE_CURVE('',#1559,#1558,#1090,.T.);
#1847=EDGE_CURVE('',#1559,#1560,#508,.T.);
#1848=EDGE_CURVE('',#1560,#1561,#509,.T.);
#1849=EDGE_CURVE('',#1555,#1561,#1091,.T.);
#1850=EDGE_CURVE('',#1562,#1546,#510,.T.);
#1851=EDGE_CURVE('',#1562,#1563,#1092,.T.);
#1852=EDGE_CURVE('',#1564,#1563,#511,.F.);
#1853=EDGE_CURVE('',#1565,#1564,#1093,.T.);
#1854=EDGE_CURVE('',#1558,#1565,#512,.T.);
#1855=EDGE_CURVE('',#1557,#1549,#1094,.T.);
#1856=EDGE_CURVE('',#1566,#1548,#513,.T.);
#1857=EDGE_CURVE('',#1566,#1567,#1095,.T.);
#1858=EDGE_CURVE('',#1568,#1567,#514,.F.);
#1859=EDGE_CURVE('',#1569,#1568,#1096,.T.);
#1860=EDGE_CURVE('',#1547,#1569,#515,.T.);
#1861=EDGE_CURVE('',#1570,#1570,#516,.T.);
#1862=EDGE_CURVE('',#1571,#1571,#517,.T.);
#1863=EDGE_CURVE('',#1572,#1573,#1097,.T.);
#1864=EDGE_CURVE('',#1574,#1573,#518,.T.);
#1865=EDGE_CURVE('',#1575,#1574,#1098,.T.);
#1866=EDGE_CURVE('',#1551,#1575,#519,.F.);
#1867=EDGE_CURVE('',#1556,#1550,#1099,.T.);
#1868=EDGE_CURVE('',#1576,#1555,#520,.F.);
#1869=EDGE_CURVE('',#1576,#1577,#1100,.T.);
#1870=EDGE_CURVE('',#1578,#1577,#521,.T.);
#1871=EDGE_CURVE('',#1579,#1578,#1101,.T.);
#1872=EDGE_CURVE('',#1544,#1579,#522,.F.);
#1873=EDGE_CURVE('',#1572,#1545,#523,.F.);
#1874=EDGE_CURVE('',#1580,#1580,#524,.T.);
#1875=EDGE_CURVE('',#1581,#1581,#525,.T.);
#1876=EDGE_CURVE('',#1570,#1580,#1102,.T.);
#1877=EDGE_CURVE('',#1571,#1581,#1103,.T.);
#1878=EDGE_CURVE('',#1553,#1560,#1104,.T.);
#1879=EDGE_CURVE('',#1561,#1559,#371,.T.);
#1880=EDGE_CURVE('',#1554,#1552,#372,.T.);
#1881=EDGE_CURVE('',#1573,#1568,#1105,.T.);
#1882=EDGE_CURVE('',#1569,#1572,#1106,.F.);
#1883=EDGE_CURVE('',#1567,#1574,#1107,.F.);
#1884=EDGE_CURVE('',#1575,#1566,#1108,.T.);
#1885=EDGE_CURVE('',#1579,#1562,#1109,.T.);
#1886=EDGE_CURVE('',#1563,#1578,#1110,.F.);
#1887=EDGE_CURVE('',#1577,#1564,#1111,.T.);
#1888=EDGE_CURVE('',#1565,#1576,#1112,.F.);
#1889=EDGE_CURVE('',#1582,#1583,#1113,.T.);
#1890=EDGE_CURVE('',#1584,#1582,#1114,.F.);
#1891=EDGE_CURVE('',#1584,#1585,#1115,.T.);
#1892=EDGE_CURVE('',#1583,#1585,#1116,.T.);
#1893=EDGE_CURVE('',#1586,#1587,#1117,.T.);
#1894=EDGE_CURVE('',#1587,#1588,#1118,.T.);
#1895=EDGE_CURVE('',#1589,#1588,#1119,.T.);
#1896=EDGE_CURVE('',#1590,#1589,#1120,.F.);
#1897=EDGE_CURVE('',#1591,#1590,#526,.T.);
#1898=EDGE_CURVE('',#1592,#1591,#527,.T.);
#1899=EDGE_CURVE('',#1586,#1592,#1121,.F.);
#1900=EDGE_CURVE('',#1593,#1594,#1122,.T.);
#1901=EDGE_CURVE('',#1595,#1594,#1123,.T.);
#1902=EDGE_CURVE('',#1596,#1595,#1124,.T.);
#1903=EDGE_CURVE('',#1597,#1596,#1125,.T.);
#1904=EDGE_CURVE('',#1597,#1598,#528,.T.);
#1905=EDGE_CURVE('',#1598,#1599,#529,.T.);
#1906=EDGE_CURVE('',#1593,#1599,#1126,.T.);
#1907=EDGE_CURVE('',#1600,#1584,#530,.T.);
#1908=EDGE_CURVE('',#1600,#1601,#1127,.T.);
#1909=EDGE_CURVE('',#1602,#1601,#531,.F.);
#1910=EDGE_CURVE('',#1603,#1602,#1128,.T.);
#1911=EDGE_CURVE('',#1596,#1603,#532,.T.);
#1912=EDGE_CURVE('',#1595,#1587,#1129,.T.);
#1913=EDGE_CURVE('',#1604,#1586,#533,.T.);
#1914=EDGE_CURVE('',#1604,#1605,#1130,.T.);
#1915=EDGE_CURVE('',#1606,#1605,#534,.F.);
#1916=EDGE_CURVE('',#1607,#1606,#1131,.T.);
#1917=EDGE_CURVE('',#1585,#1607,#535,.T.);
#1918=EDGE_CURVE('',#1608,#1608,#536,.T.);
#1919=EDGE_CURVE('',#1609,#1609,#537,.T.);
#1920=EDGE_CURVE('',#1610,#1611,#1132,.T.);
#1921=EDGE_CURVE('',#1612,#1611,#538,.T.);
#1922=EDGE_CURVE('',#1613,#1612,#1133,.T.);
#1923=EDGE_CURVE('',#1589,#1613,#539,.F.);
#1924=EDGE_CURVE('',#1594,#1588,#1134,.T.);
#1925=EDGE_CURVE('',#1614,#1593,#540,.F.);
#1926=EDGE_CURVE('',#1614,#1615,#1135,.T.);
#1927=EDGE_CURVE('',#1616,#1615,#541,.T.);
#1928=EDGE_CURVE('',#1617,#1616,#1136,.T.);
#1929=EDGE_CURVE('',#1582,#1617,#542,.F.);
#1930=EDGE_CURVE('',#1610,#1583,#543,.F.);
#1931=EDGE_CURVE('',#1618,#1618,#544,.T.);
#1932=EDGE_CURVE('',#1619,#1619,#545,.T.);
#1933=EDGE_CURVE('',#1608,#1618,#1137,.T.);
#1934=EDGE_CURVE('',#1609,#1619,#1138,.T.);
#1935=EDGE_CURVE('',#1591,#1598,#1139,.T.);
#1936=EDGE_CURVE('',#1599,#1597,#373,.T.);
#1937=EDGE_CURVE('',#1592,#1590,#374,.T.);
#1938=EDGE_CURVE('',#1611,#1606,#1140,.T.);
#1939=EDGE_CURVE('',#1607,#1610,#1141,.F.);
#1940=EDGE_CURVE('',#1605,#1612,#1142,.F.);
#1941=EDGE_CURVE('',#1613,#1604,#1143,.T.);
#1942=EDGE_CURVE('',#1617,#1600,#1144,.T.);
#1943=EDGE_CURVE('',#1601,#1616,#1145,.F.);
#1944=EDGE_CURVE('',#1615,#1602,#1146,.T.);
#1945=EDGE_CURVE('',#1603,#1614,#1147,.F.);
#1946=EDGE_CURVE('',#1620,#1621,#1148,.T.);
#1947=EDGE_CURVE('',#1621,#1622,#1149,.T.);
#1948=EDGE_CURVE('',#1623,#1622,#1150,.T.);
#1949=EDGE_CURVE('',#1623,#1620,#1151,.F.);
#1950=EDGE_CURVE('',#1624,#1625,#1152,.T.);
#1951=EDGE_CURVE('',#1624,#1626,#1153,.F.);
#1952=EDGE_CURVE('',#1626,#1627,#546,.T.);
#1953=EDGE_CURVE('',#1627,#1628,#547,.T.);
#1954=EDGE_CURVE('',#1628,#1629,#1154,.F.);
#1955=EDGE_CURVE('',#1629,#1630,#1155,.T.);
#1956=EDGE_CURVE('',#1625,#1630,#1156,.T.);
#1957=EDGE_CURVE('',#1631,#1632,#1157,.T.);
#1958=EDGE_CURVE('',#1631,#1633,#1158,.T.);
#1959=EDGE_CURVE('',#1634,#1633,#548,.T.);
#1960=EDGE_CURVE('',#1635,#1634,#549,.T.);
#1961=EDGE_CURVE('',#1635,#1636,#1159,.T.);
#1962=EDGE_CURVE('',#1636,#1637,#1160,.T.);
#1963=EDGE_CURVE('',#1637,#1632,#1161,.T.);
#1964=EDGE_CURVE('',#1622,#1638,#550,.T.);
#1965=EDGE_CURVE('',#1638,#1639,#1162,.T.);
#1966=EDGE_CURVE('',#1639,#1640,#551,.F.);
#1967=EDGE_CURVE('',#1641,#1640,#1163,.T.);
#1968=EDGE_CURVE('',#1641,#1624,#552,.T.);
#1969=EDGE_CURVE('',#1637,#1625,#1164,.T.);
#1970=EDGE_CURVE('',#1636,#1642,#553,.T.);
#1971=EDGE_CURVE('',#1642,#1643,#1165,.T.);
#1972=EDGE_CURVE('',#1643,#1644,#554,.F.);
#1973=EDGE_CURVE('',#1645,#1644,#1166,.T.);
#1974=EDGE_CURVE('',#1645,#1623,#555,.T.);
#1975=EDGE_CURVE('',#1646,#1646,#556,.T.);
#1976=EDGE_CURVE('',#1647,#1647,#557,.T.);
#1977=EDGE_CURVE('',#1648,#1649,#1167,.T.);
#1978=EDGE_CURVE('',#1648,#1621,#558,.F.);
#1979=EDGE_CURVE('',#1620,#1650,#559,.F.);
#1980=EDGE_CURVE('',#1650,#1651,#1168,.T.);
#1981=EDGE_CURVE('',#1651,#1652,#560,.T.);
#1982=EDGE_CURVE('',#1653,#1652,#1169,.T.);
#1983=EDGE_CURVE('',#1653,#1631,#561,.F.);
#1984=EDGE_CURVE('',#1632,#1630,#1170,.T.);
#1985=EDGE_CURVE('',#1629,#1654,#562,.F.);
#1986=EDGE_CURVE('',#1654,#1655,#1171,.T.);
#1987=EDGE_CURVE('',#1655,#1649,#563,.T.);
#1988=EDGE_CURVE('',#1656,#1656,#564,.T.);
#1989=EDGE_CURVE('',#1657,#1657,#565,.T.);
#1990=EDGE_CURVE('',#1646,#1656,#1172,.T.);
#1991=EDGE_CURVE('',#1647,#1657,#1173,.T.);
#1992=EDGE_CURVE('',#1626,#1628,#375,.T.);
#1993=EDGE_CURVE('',#1627,#1634,#1174,.T.);
#1994=EDGE_CURVE('',#1633,#1635,#376,.T.);
#1995=EDGE_CURVE('',#1638,#1648,#1175,.F.);
#1996=EDGE_CURVE('',#1649,#1639,#1176,.T.);
#1997=EDGE_CURVE('',#1654,#1641,#1177,.T.);
#1998=EDGE_CURVE('',#1640,#1655,#1178,.F.);
#1999=EDGE_CURVE('',#1644,#1651,#1179,.F.);
#2000=EDGE_CURVE('',#1650,#1645,#1180,.T.);
#2001=EDGE_CURVE('',#1642,#1653,#1181,.F.);
#2002=EDGE_CURVE('',#1652,#1643,#1182,.T.);
#2003=EDGE_CURVE('',#1658,#1659,#1183,.T.);
#2004=EDGE_CURVE('',#1659,#1660,#1184,.T.);
#2005=EDGE_CURVE('',#1661,#1660,#1185,.T.);
#2006=EDGE_CURVE('',#1661,#1658,#1186,.F.);
#2007=EDGE_CURVE('',#1662,#1663,#1187,.T.);
#2008=EDGE_CURVE('',#1662,#1664,#1188,.F.);
#2009=EDGE_CURVE('',#1664,#1665,#566,.T.);
#2010=EDGE_CURVE('',#1665,#1666,#567,.T.);
#2011=EDGE_CURVE('',#1666,#1667,#1189,.F.);
#2012=EDGE_CURVE('',#1667,#1668,#1190,.T.);
#2013=EDGE_CURVE('',#1663,#1668,#1191,.T.);
#2014=EDGE_CURVE('',#1669,#1670,#1192,.T.);
#2015=EDGE_CURVE('',#1669,#1671,#1193,.T.);
#2016=EDGE_CURVE('',#1672,#1671,#568,.T.);
#2017=EDGE_CURVE('',#1673,#1672,#569,.T.);
#2018=EDGE_CURVE('',#1673,#1674,#1194,.T.);
#2019=EDGE_CURVE('',#1674,#1675,#1195,.T.);
#2020=EDGE_CURVE('',#1675,#1670,#1196,.T.);
#2021=EDGE_CURVE('',#1660,#1676,#570,.T.);
#2022=EDGE_CURVE('',#1676,#1677,#1197,.T.);
#2023=EDGE_CURVE('',#1677,#1678,#571,.F.);
#2024=EDGE_CURVE('',#1679,#1678,#1198,.T.);
#2025=EDGE_CURVE('',#1679,#1662,#572,.T.);
#2026=EDGE_CURVE('',#1675,#1663,#1199,.T.);
#2027=EDGE_CURVE('',#1674,#1680,#573,.T.);
#2028=EDGE_CURVE('',#1680,#1681,#1200,.T.);
#2029=EDGE_CURVE('',#1681,#1682,#574,.F.);
#2030=EDGE_CURVE('',#1683,#1682,#1201,.T.);
#2031=EDGE_CURVE('',#1683,#1661,#575,.T.);
#2032=EDGE_CURVE('',#1684,#1684,#576,.T.);
#2033=EDGE_CURVE('',#1685,#1685,#577,.T.);
#2034=EDGE_CURVE('',#1686,#1687,#1202,.T.);
#2035=EDGE_CURVE('',#1686,#1659,#578,.F.);
#2036=EDGE_CURVE('',#1658,#1688,#579,.F.);
#2037=EDGE_CURVE('',#1688,#1689,#1203,.T.);
#2038=EDGE_CURVE('',#1689,#1690,#580,.T.);
#2039=EDGE_CURVE('',#1691,#1690,#1204,.T.);
#2040=EDGE_CURVE('',#1691,#1669,#581,.F.);
#2041=EDGE_CURVE('',#1670,#1668,#1205,.T.);
#2042=EDGE_CURVE('',#1667,#1692,#582,.F.);
#2043=EDGE_CURVE('',#1692,#1693,#1206,.T.);
#2044=EDGE_CURVE('',#1693,#1687,#583,.T.);
#2045=EDGE_CURVE('',#1694,#1694,#584,.T.);
#2046=EDGE_CURVE('',#1695,#1695,#585,.T.);
#2047=EDGE_CURVE('',#1684,#1694,#1207,.T.);
#2048=EDGE_CURVE('',#1685,#1695,#1208,.T.);
#2049=EDGE_CURVE('',#1664,#1666,#377,.T.);
#2050=EDGE_CURVE('',#1665,#1672,#1209,.T.);
#2051=EDGE_CURVE('',#1671,#1673,#378,.T.);
#2052=EDGE_CURVE('',#1676,#1686,#1210,.F.);
#2053=EDGE_CURVE('',#1687,#1677,#1211,.T.);
#2054=EDGE_CURVE('',#1692,#1679,#1212,.T.);
#2055=EDGE_CURVE('',#1678,#1693,#1213,.F.);
#2056=EDGE_CURVE('',#1682,#1689,#1214,.F.);
#2057=EDGE_CURVE('',#1688,#1683,#1215,.T.);
#2058=EDGE_CURVE('',#1680,#1691,#1216,.F.);
#2059=EDGE_CURVE('',#1690,#1681,#1217,.T.);
#2060=EDGE_CURVE('',#1696,#1697,#1218,.T.);
#2061=EDGE_CURVE('',#1698,#1697,#1219,.T.);
#2062=EDGE_CURVE('',#1699,#1698,#1220,.T.);
#2063=EDGE_CURVE('',#1696,#1699,#1221,.F.);
#2064=EDGE_CURVE('',#1700,#1701,#1222,.T.);
#2065=EDGE_CURVE('',#1702,#1700,#1223,.F.);
#2066=EDGE_CURVE('',#1702,#1703,#1224,.T.);
#2067=EDGE_CURVE('',#1701,#1703,#1225,.T.);
#2068=EDGE_CURVE('',#1704,#1705,#1226,.T.);
#2069=EDGE_CURVE('',#1706,#1705,#1227,.F.);
#2070=EDGE_CURVE('',#1707,#1706,#1228,.T.);
#2071=EDGE_CURVE('',#1704,#1707,#1229,.T.);
#2072=EDGE_CURVE('',#1708,#1708,#586,.T.);
#2073=EDGE_CURVE('',#1709,#1709,#587,.T.);
#2074=EDGE_CURVE('',#1710,#1711,#1230,.T.);
#2075=EDGE_CURVE('',#1712,#1711,#1231,.F.);
#2076=EDGE_CURVE('',#1713,#1712,#1232,.T.);
#2077=EDGE_CURVE('',#1710,#1713,#1233,.T.);
#2078=EDGE_CURVE('',#1714,#1714,#588,.T.);
#2079=EDGE_CURVE('',#1714,#1715,#1234,.T.);
#2080=EDGE_CURVE('',#1715,#1715,#589,.T.);
#2081=EDGE_CURVE('',#1716,#1717,#1235,.T.);
#2082=EDGE_CURVE('',#1718,#1716,#1236,.F.);
#2083=EDGE_CURVE('',#1718,#1719,#1237,.T.);
#2084=EDGE_CURVE('',#1717,#1719,#1238,.T.);
#2085=EDGE_CURVE('',#1720,#1720,#590,.T.);
#2086=EDGE_CURVE('',#1720,#1721,#1239,.T.);
#2087=EDGE_CURVE('',#1721,#1721,#591,.T.);
#2088=EDGE_CURVE('',#1722,#1723,#1240,.T.);
#2089=EDGE_CURVE('',#1724,#1722,#592,.F.);
#2090=EDGE_CURVE('',#1719,#1724,#593,.T.);
#2091=EDGE_CURVE('',#1703,#1718,#594,.F.);
#2092=EDGE_CURVE('',#1707,#1702,#595,.F.);
#2093=EDGE_CURVE('',#1713,#1706,#596,.F.);
#2094=EDGE_CURVE('',#1697,#1712,#597,.F.);
#2095=EDGE_CURVE('',#1725,#1696,#598,.T.);
#2096=EDGE_CURVE('',#1723,#1725,#599,.F.);
#2097=EDGE_CURVE('',#1711,#1698,#600,.T.);
#2098=EDGE_CURVE('',#1705,#1710,#601,.T.);
#2099=EDGE_CURVE('',#1700,#1704,#602,.T.);
#2100=EDGE_CURVE('',#1716,#1701,#603,.T.);
#2101=EDGE_CURVE('',#1726,#1717,#604,.F.);
#2102=EDGE_CURVE('',#1727,#1726,#605,.T.);
#2103=EDGE_CURVE('',#1727,#1728,#1241,.T.);
#2104=EDGE_CURVE('',#1729,#1728,#606,.T.);
#2105=EDGE_CURVE('',#1699,#1729,#607,.F.);
#2106=EDGE_CURVE('',#1730,#1727,#1242,.F.);
#2107=EDGE_CURVE('',#1730,#1731,#608,.T.);
#2108=EDGE_CURVE('',#1722,#1731,#1243,.F.);
#2109=EDGE_CURVE('',#1732,#1723,#1244,.T.);
#2110=EDGE_CURVE('',#1732,#1733,#609,.T.);
#2111=EDGE_CURVE('',#1733,#1734,#610,.T.);
#2112=EDGE_CURVE('',#1728,#1734,#1245,.T.);
#2113=EDGE_CURVE('',#1709,#1735,#1246,.T.);
#2114=EDGE_CURVE('',#1731,#1735,#379,.T.);
#2115=EDGE_CURVE('',#1735,#1730,#380,.T.);
#2116=EDGE_CURVE('',#1708,#1733,#1247,.T.);
#2117=EDGE_CURVE('',#1734,#1732,#381,.T.);
#2118=EDGE_CURVE('',#1725,#1729,#1248,.F.);
#2119=EDGE_CURVE('',#1726,#1724,#1249,.T.);
#2120=EDGE_CURVE('',#1736,#1737,#1250,.T.);
#2121=EDGE_CURVE('',#1736,#1738,#1251,.F.);
#2122=EDGE_CURVE('',#1738,#1739,#1252,.T.);
#2123=EDGE_CURVE('',#1739,#1737,#1253,.T.);
#2124=EDGE_CURVE('',#1740,#1741,#1254,.T.);
#2125=EDGE_CURVE('',#1741,#1742,#1255,.T.);
#2126=EDGE_CURVE('',#1743,#1742,#1256,.T.);
#2127=EDGE_CURVE('',#1743,#1740,#1257,.F.);
#2128=EDGE_CURVE('',#1744,#1745,#1258,.T.);
#2129=EDGE_CURVE('',#1744,#1746,#1259,.T.);
#2130=EDGE_CURVE('',#1746,#1747,#1260,.T.);
#2131=EDGE_CURVE('',#1747,#1745,#1261,.F.);
#2132=EDGE_CURVE('',#1748,#1748,#611,.T.);
#2133=EDGE_CURVE('',#1749,#1749,#612,.T.);
#2134=EDGE_CURVE('',#1750,#1751,#1262,.T.);
#2135=EDGE_CURVE('',#1750,#1752,#1263,.T.);
#2136=EDGE_CURVE('',#1752,#1753,#1264,.T.);
#2137=EDGE_CURVE('',#1753,#1751,#1265,.F.);
#2138=EDGE_CURVE('',#1754,#1754,#613,.T.);
#2139=EDGE_CURVE('',#1754,#1755,#1266,.T.);
#2140=EDGE_CURVE('',#1755,#1755,#614,.T.);
#2141=EDGE_CURVE('',#1756,#1757,#1267,.T.);
#2142=EDGE_CURVE('',#1757,#1758,#1268,.T.);
#2143=EDGE_CURVE('',#1759,#1758,#1269,.T.);
#2144=EDGE_CURVE('',#1759,#1756,#1270,.F.);
#2145=EDGE_CURVE('',#1760,#1760,#615,.T.);
#2146=EDGE_CURVE('',#1760,#1761,#1271,.T.);
#2147=EDGE_CURVE('',#1761,#1761,#616,.T.);
#2148=EDGE_CURVE('',#1762,#1763,#1272,.T.);
#2149=EDGE_CURVE('',#1763,#1764,#617,.F.);
#2150=EDGE_CURVE('',#1764,#1736,#618,.T.);
#2151=EDGE_CURVE('',#1737,#1753,#619,.F.);
#2152=EDGE_CURVE('',#1752,#1747,#620,.F.);
#2153=EDGE_CURVE('',#1746,#1743,#621,.F.);
#2154=EDGE_CURVE('',#1742,#1759,#622,.F.);
#2155=EDGE_CURVE('',#1758,#1765,#623,.T.);
#2156=EDGE_CURVE('',#1765,#1762,#624,.F.);
#2157=EDGE_CURVE('',#1738,#1766,#625,.F.);
#2158=EDGE_CURVE('',#1766,#1767,#626,.T.);
#2159=EDGE_CURVE('',#1768,#1767,#1273,.T.);
#2160=EDGE_CURVE('',#1768,#1769,#627,.T.);
#2161=EDGE_CURVE('',#1769,#1757,#628,.F.);
#2162=EDGE_CURVE('',#1756,#1741,#629,.T.);
#2163=EDGE_CURVE('',#1740,#1744,#630,.T.);
#2164=EDGE_CURVE('',#1745,#1750,#631,.T.);
#2165=EDGE_CURVE('',#1751,#1739,#632,.T.);
#2166=EDGE_CURVE('',#1767,#1770,#1274,.T.);
#2167=EDGE_CURVE('',#1771,#1770,#633,.T.);
#2168=EDGE_CURVE('',#1772,#1771,#634,.T.);
#2169=EDGE_CURVE('',#1772,#1763,#1275,.T.);
#2170=EDGE_CURVE('',#1762,#1773,#1276,.F.);
#2171=EDGE_CURVE('',#1774,#1773,#635,.T.);
#2172=EDGE_CURVE('',#1774,#1768,#1277,.F.);
#2173=EDGE_CURVE('',#1749,#1775,#1278,.T.);
#2174=EDGE_CURVE('',#1775,#1774,#382,.F.);
#2175=EDGE_CURVE('',#1773,#1775,#383,.F.);
#2176=EDGE_CURVE('',#1748,#1771,#1279,.T.);
#2177=EDGE_CURVE('',#1770,#1772,#384,.T.);
#2178=EDGE_CURVE('',#1764,#1766,#1280,.F.);
#2179=EDGE_CURVE('',#1769,#1765,#1281,.T.);
#2180=EDGE_CURVE('',#1776,#1777,#636,.T.);
#2181=EDGE_CURVE('',#1777,#1778,#1282,.T.);
#2182=EDGE_CURVE('',#1778,#1779,#637,.F.);
#2183=EDGE_CURVE('',#1779,#1778,#638,.F.);
#2184=EDGE_CURVE('',#1777,#1776,#639,.T.);
#2185=EDGE_CURVE('',#1780,#1780,#640,.T.);
#2186=EDGE_CURVE('',#1781,#1781,#641,.F.);
#2187=EDGE_CURVE('',#1776,#1781,#642,.T.);
#2188=EDGE_CURVE('',#1780,#1779,#643,.T.);
#2189=EDGE_CURVE('',#1782,#1783,#644,.T.);
#2190=EDGE_CURVE('',#1783,#1784,#1283,.T.);
#2191=EDGE_CURVE('',#1784,#1784,#645,.T.);
#2192=EDGE_CURVE('',#1783,#1782,#646,.T.);
#2193=EDGE_CURVE('',#1785,#1785,#647,.T.);
#2194=EDGE_CURVE('',#1782,#1786,#1284,.T.);
#2195=EDGE_CURVE('',#1786,#1786,#648,.T.);
#2196=EDGE_CURVE('',#1787,#1788,#649,.T.);
#2197=EDGE_CURVE('',#1788,#1785,#1285,.T.);
#2198=EDGE_CURVE('',#1788,#1787,#650,.T.);
#2199=EDGE_CURVE('',#1789,#1789,#651,.T.);
#2200=EDGE_CURVE('',#1789,#1787,#1286,.T.);
#2201=EDGE_CURVE('',#1790,#1791,#652,.T.);
#2202=EDGE_CURVE('',#1791,#1792,#1287,.T.);
#2203=EDGE_CURVE('',#1792,#1792,#653,.T.);
#2204=EDGE_CURVE('',#1791,#1790,#654,.T.);
#2205=EDGE_CURVE('',#1793,#1793,#655,.T.);
#2206=EDGE_CURVE('',#1794,#1794,#656,.T.);
#2207=EDGE_CURVE('',#1794,#1790,#1288,.T.);
#2208=EDGE_CURVE('',#1795,#1796,#657,.T.);
#2209=EDGE_CURVE('',#1796,#1793,#1289,.T.);
#2210=EDGE_CURVE('',#1796,#1795,#658,.T.);
#2211=EDGE_CURVE('',#1795,#1797,#1290,.T.);
#2212=EDGE_CURVE('',#1797,#1797,#659,.T.);
#2213=EDGE_CURVE('',#1798,#1798,#660,.T.);
#2214=EDGE_CURVE('',#1799,#1799,#661,.T.);
#2215=EDGE_CURVE('',#1799,#1798,#1291,.T.);
#2216=EDGE_CURVE('',#1800,#1800,#662,.T.);
#2217=EDGE_CURVE('',#1801,#1801,#663,.T.);
#2218=EDGE_CURVE('',#1801,#1800,#1292,.T.);
#2219=EDGE_CURVE('',#1802,#1802,#664,.T.);
#2220=EDGE_CURVE('',#1802,#1801,#1293,.T.);
#2221=EDGE_CURVE('',#1803,#1803,#665,.T.);
#2222=EDGE_CURVE('',#1803,#1802,#1294,.T.);
#2223=EDGE_CURVE('',#1803,#1804,#1295,.T.);
#2224=EDGE_CURVE('',#1804,#1804,#666,.T.);
#2225=EDGE_CURVE('',#1805,#1805,#667,.T.);
#2226=EDGE_CURVE('',#1805,#1804,#1296,.T.);
#2227=EDGE_CURVE('',#1806,#1806,#668,.T.);
#2228=EDGE_CURVE('',#1807,#1807,#669,.T.);
#2229=EDGE_CURVE('',#1807,#1806,#1297,.T.);
#2230=EDGE_CURVE('',#1808,#1808,#670,.T.);
#2231=EDGE_CURVE('',#1809,#1809,#671,.T.);
#2232=EDGE_CURVE('',#1809,#1808,#1298,.T.);
#2233=EDGE_CURVE('',#1810,#1810,#672,.T.);
#2234=EDGE_CURVE('',#1811,#1811,#673,.T.);
#2235=EDGE_CURVE('',#1811,#1810,#1299,.T.);
#2236=EDGE_CURVE('',#1812,#1812,#674,.T.);
#2237=EDGE_CURVE('',#1813,#1813,#675,.T.);
#2238=EDGE_CURVE('',#1813,#1812,#1300,.T.);
#2239=EDGE_CURVE('',#1814,#1814,#676,.T.);
#2240=EDGE_CURVE('',#1815,#1815,#677,.T.);
#2241=EDGE_CURVE('',#1814,#1816,#1301,.T.);
#2242=EDGE_CURVE('',#1816,#1816,#678,.T.);
#2243=EDGE_CURVE('',#1817,#1817,#679,.T.);
#2244=EDGE_CURVE('',#1818,#1818,#680,.T.);
#2245=EDGE_CURVE('',#1818,#1817,#1302,.T.);
#2246=EDGE_CURVE('',#1818,#1819,#1303,.T.);
#2247=EDGE_CURVE('',#1819,#1819,#681,.T.);
#2248=EDGE_CURVE('',#1820,#1820,#682,.T.);
#2249=EDGE_CURVE('',#1815,#1820,#1304,.T.);
#2250=EDGE_CURVE('',#1821,#1821,#683,.T.);
#2251=EDGE_CURVE('',#1822,#1822,#684,.T.);
#2252=EDGE_CURVE('',#1823,#1823,#685,.T.);
#2253=EDGE_CURVE('',#1823,#1821,#1305,.T.);
#2254=EDGE_CURVE('',#1824,#1824,#686,.T.);
#2255=EDGE_CURVE('',#1825,#1825,#687,.T.);
#2256=EDGE_CURVE('',#1825,#1824,#1306,.T.);
#2257=EDGE_CURVE('',#1826,#1826,#688,.T.);
#2258=EDGE_CURVE('',#1826,#1825,#1307,.T.);
#2259=EDGE_CURVE('',#1827,#1827,#689,.T.);
#2260=EDGE_CURVE('',#1822,#1827,#1308,.T.);
#2261=EDGE_CURVE('',#1828,#1828,#690,.T.);
#2262=EDGE_CURVE('',#1829,#1829,#691,.T.);
#2263=EDGE_CURVE('',#1828,#1830,#1309,.T.);
#2264=EDGE_CURVE('',#1830,#1830,#692,.T.);
#2265=EDGE_CURVE('',#1831,#1831,#693,.T.);
#2266=EDGE_CURVE('',#1831,#1829,#1310,.T.);
#2267=ORIENTED_EDGE('',*,*,#1832,.F.);
#2268=ORIENTED_EDGE('',*,*,#1833,.F.);
#2269=ORIENTED_EDGE('',*,*,#1834,.T.);
#2270=ORIENTED_EDGE('',*,*,#1835,.F.);
#2271=ORIENTED_EDGE('',*,*,#1836,.T.);
#2272=ORIENTED_EDGE('',*,*,#1837,.T.);
#2273=ORIENTED_EDGE('',*,*,#1838,.F.);
#2274=ORIENTED_EDGE('',*,*,#1839,.F.);
#2275=ORIENTED_EDGE('',*,*,#1840,.F.);
#2276=ORIENTED_EDGE('',*,*,#1841,.F.);
#2277=ORIENTED_EDGE('',*,*,#1842,.F.);
#2278=ORIENTED_EDGE('',*,*,#1843,.T.);
#2279=ORIENTED_EDGE('',*,*,#1844,.F.);
#2280=ORIENTED_EDGE('',*,*,#1845,.F.);
#2281=ORIENTED_EDGE('',*,*,#1846,.F.);
#2282=ORIENTED_EDGE('',*,*,#1847,.T.);
#2283=ORIENTED_EDGE('',*,*,#1848,.T.);
#2284=ORIENTED_EDGE('',*,*,#1849,.F.);
#2285=ORIENTED_EDGE('',*,*,#1834,.F.);
#2286=ORIENTED_EDGE('',*,*,#1850,.F.);
#2287=ORIENTED_EDGE('',*,*,#1851,.T.);
#2288=ORIENTED_EDGE('',*,*,#1852,.F.);
#2289=ORIENTED_EDGE('',*,*,#1853,.F.);
#2290=ORIENTED_EDGE('',*,*,#1854,.F.);
#2291=ORIENTED_EDGE('',*,*,#1845,.T.);
#2292=ORIENTED_EDGE('',*,*,#1855,.T.);
#2293=ORIENTED_EDGE('',*,*,#1836,.F.);
#2294=ORIENTED_EDGE('',*,*,#1856,.F.);
#2295=ORIENTED_EDGE('',*,*,#1857,.T.);
#2296=ORIENTED_EDGE('',*,*,#1858,.F.);
#2297=ORIENTED_EDGE('',*,*,#1859,.F.);
#2298=ORIENTED_EDGE('',*,*,#1860,.F.);
#2299=ORIENTED_EDGE('',*,*,#1861,.T.);
#2300=ORIENTED_EDGE('',*,*,#1862,.T.);
#2301=ORIENTED_EDGE('',*,*,#1863,.T.);
#2302=ORIENTED_EDGE('',*,*,#1864,.F.);
#2303=ORIENTED_EDGE('',*,*,#1865,.F.);
#2304=ORIENTED_EDGE('',*,*,#1866,.F.);
#2305=ORIENTED_EDGE('',*,*,#1838,.T.);
#2306=ORIENTED_EDGE('',*,*,#1867,.F.);
#2307=ORIENTED_EDGE('',*,*,#1843,.F.);
#2308=ORIENTED_EDGE('',*,*,#1868,.F.);
#2309=ORIENTED_EDGE('',*,*,#1869,.T.);
#2310=ORIENTED_EDGE('',*,*,#1870,.F.);
#2311=ORIENTED_EDGE('',*,*,#1871,.F.);
#2312=ORIENTED_EDGE('',*,*,#1872,.F.);
#2313=ORIENTED_EDGE('',*,*,#1832,.T.);
#2314=ORIENTED_EDGE('',*,*,#1873,.F.);
#2315=ORIENTED_EDGE('',*,*,#1874,.F.);
#2316=ORIENTED_EDGE('',*,*,#1875,.F.);
#2317=ORIENTED_EDGE('',*,*,#1861,.F.);
#2318=ORIENTED_EDGE('',*,*,#1876,.T.);
#2319=ORIENTED_EDGE('',*,*,#1874,.T.);
#2320=ORIENTED_EDGE('',*,*,#1876,.F.);
#2321=ORIENTED_EDGE('',*,*,#1862,.F.);
#2322=ORIENTED_EDGE('',*,*,#1877,.T.);
#2323=ORIENTED_EDGE('',*,*,#1875,.T.);
#2324=ORIENTED_EDGE('',*,*,#1877,.F.);
#2325=ORIENTED_EDGE('',*,*,#1867,.T.);
#2326=ORIENTED_EDGE('',*,*,#1837,.F.);
#2327=ORIENTED_EDGE('',*,*,#1855,.F.);
#2328=ORIENTED_EDGE('',*,*,#1844,.T.);
#2329=ORIENTED_EDGE('',*,*,#1841,.T.);
#2330=ORIENTED_EDGE('',*,*,#1878,.T.);
#2331=ORIENTED_EDGE('',*,*,#1847,.F.);
#2332=ORIENTED_EDGE('',*,*,#1879,.F.);
#2333=ORIENTED_EDGE('',*,*,#1848,.F.);
#2334=ORIENTED_EDGE('',*,*,#1878,.F.);
#2335=ORIENTED_EDGE('',*,*,#1840,.T.);
#2336=ORIENTED_EDGE('',*,*,#1880,.F.);
#2337=ORIENTED_EDGE('',*,*,#1859,.T.);
#2338=ORIENTED_EDGE('',*,*,#1881,.F.);
#2339=ORIENTED_EDGE('',*,*,#1863,.F.);
#2340=ORIENTED_EDGE('',*,*,#1882,.F.);
#2341=ORIENTED_EDGE('',*,*,#1865,.T.);
#2342=ORIENTED_EDGE('',*,*,#1883,.F.);
#2343=ORIENTED_EDGE('',*,*,#1857,.F.);
#2344=ORIENTED_EDGE('',*,*,#1884,.F.);
#2345=ORIENTED_EDGE('',*,*,#1851,.F.);
#2346=ORIENTED_EDGE('',*,*,#1885,.F.);
#2347=ORIENTED_EDGE('',*,*,#1871,.T.);
#2348=ORIENTED_EDGE('',*,*,#1886,.F.);
#2349=ORIENTED_EDGE('',*,*,#1853,.T.);
#2350=ORIENTED_EDGE('',*,*,#1887,.F.);
#2351=ORIENTED_EDGE('',*,*,#1869,.F.);
#2352=ORIENTED_EDGE('',*,*,#1888,.F.);
#2353=ORIENTED_EDGE('',*,*,#1873,.T.);
#2354=ORIENTED_EDGE('',*,*,#1835,.T.);
#2355=ORIENTED_EDGE('',*,*,#1860,.T.);
#2356=ORIENTED_EDGE('',*,*,#1882,.T.);
#2357=ORIENTED_EDGE('',*,*,#1880,.T.);
#2358=ORIENTED_EDGE('',*,*,#1839,.T.);
#2359=ORIENTED_EDGE('',*,*,#1866,.T.);
#2360=ORIENTED_EDGE('',*,*,#1884,.T.);
#2361=ORIENTED_EDGE('',*,*,#1856,.T.);
#2362=ORIENTED_EDGE('',*,*,#1842,.T.);
#2363=ORIENTED_EDGE('',*,*,#1864,.T.);
#2364=ORIENTED_EDGE('',*,*,#1881,.T.);
#2365=ORIENTED_EDGE('',*,*,#1858,.T.);
#2366=ORIENTED_EDGE('',*,*,#1883,.T.);
#2367=ORIENTED_EDGE('',*,*,#1868,.T.);
#2368=ORIENTED_EDGE('',*,*,#1849,.T.);
#2369=ORIENTED_EDGE('',*,*,#1879,.T.);
#2370=ORIENTED_EDGE('',*,*,#1846,.T.);
#2371=ORIENTED_EDGE('',*,*,#1854,.T.);
#2372=ORIENTED_EDGE('',*,*,#1888,.T.);
#2373=ORIENTED_EDGE('',*,*,#1870,.T.);
#2374=ORIENTED_EDGE('',*,*,#1887,.T.);
#2375=ORIENTED_EDGE('',*,*,#1852,.T.);
#2376=ORIENTED_EDGE('',*,*,#1886,.T.);
#2377=ORIENTED_EDGE('',*,*,#1872,.T.);
#2378=ORIENTED_EDGE('',*,*,#1885,.T.);
#2379=ORIENTED_EDGE('',*,*,#1850,.T.);
#2380=ORIENTED_EDGE('',*,*,#1833,.T.);
#2381=ORIENTED_EDGE('',*,*,#1889,.F.);
#2382=ORIENTED_EDGE('',*,*,#1890,.F.);
#2383=ORIENTED_EDGE('',*,*,#1891,.T.);
#2384=ORIENTED_EDGE('',*,*,#1892,.F.);
#2385=ORIENTED_EDGE('',*,*,#1893,.T.);
#2386=ORIENTED_EDGE('',*,*,#1894,.T.);
#2387=ORIENTED_EDGE('',*,*,#1895,.F.);
#2388=ORIENTED_EDGE('',*,*,#1896,.F.);
#2389=ORIENTED_EDGE('',*,*,#1897,.F.);
#2390=ORIENTED_EDGE('',*,*,#1898,.F.);
#2391=ORIENTED_EDGE('',*,*,#1899,.F.);
#2392=ORIENTED_EDGE('',*,*,#1900,.T.);
#2393=ORIENTED_EDGE('',*,*,#1901,.F.);
#2394=ORIENTED_EDGE('',*,*,#1902,.F.);
#2395=ORIENTED_EDGE('',*,*,#1903,.F.);
#2396=ORIENTED_EDGE('',*,*,#1904,.T.);
#2397=ORIENTED_EDGE('',*,*,#1905,.T.);
#2398=ORIENTED_EDGE('',*,*,#1906,.F.);
#2399=ORIENTED_EDGE('',*,*,#1891,.F.);
#2400=ORIENTED_EDGE('',*,*,#1907,.F.);
#2401=ORIENTED_EDGE('',*,*,#1908,.T.);
#2402=ORIENTED_EDGE('',*,*,#1909,.F.);
#2403=ORIENTED_EDGE('',*,*,#1910,.F.);
#2404=ORIENTED_EDGE('',*,*,#1911,.F.);
#2405=ORIENTED_EDGE('',*,*,#1902,.T.);
#2406=ORIENTED_EDGE('',*,*,#1912,.T.);
#2407=ORIENTED_EDGE('',*,*,#1893,.F.);
#2408=ORIENTED_EDGE('',*,*,#1913,.F.);
#2409=ORIENTED_EDGE('',*,*,#1914,.T.);
#2410=ORIENTED_EDGE('',*,*,#1915,.F.);
#2411=ORIENTED_EDGE('',*,*,#1916,.F.);
#2412=ORIENTED_EDGE('',*,*,#1917,.F.);
#2413=ORIENTED_EDGE('',*,*,#1918,.T.);
#2414=ORIENTED_EDGE('',*,*,#1919,.T.);
#2415=ORIENTED_EDGE('',*,*,#1920,.T.);
#2416=ORIENTED_EDGE('',*,*,#1921,.F.);
#2417=ORIENTED_EDGE('',*,*,#1922,.F.);
#2418=ORIENTED_EDGE('',*,*,#1923,.F.);
#2419=ORIENTED_EDGE('',*,*,#1895,.T.);
#2420=ORIENTED_EDGE('',*,*,#1924,.F.);
#2421=ORIENTED_EDGE('',*,*,#1900,.F.);
#2422=ORIENTED_EDGE('',*,*,#1925,.F.);
#2423=ORIENTED_EDGE('',*,*,#1926,.T.);
#2424=ORIENTED_EDGE('',*,*,#1927,.F.);
#2425=ORIENTED_EDGE('',*,*,#1928,.F.);
#2426=ORIENTED_EDGE('',*,*,#1929,.F.);
#2427=ORIENTED_EDGE('',*,*,#1889,.T.);
#2428=ORIENTED_EDGE('',*,*,#1930,.F.);
#2429=ORIENTED_EDGE('',*,*,#1931,.F.);
#2430=ORIENTED_EDGE('',*,*,#1932,.F.);
#2431=ORIENTED_EDGE('',*,*,#1918,.F.);
#2432=ORIENTED_EDGE('',*,*,#1933,.T.);
#2433=ORIENTED_EDGE('',*,*,#1931,.T.);
#2434=ORIENTED_EDGE('',*,*,#1933,.F.);
#2435=ORIENTED_EDGE('',*,*,#1919,.F.);
#2436=ORIENTED_EDGE('',*,*,#1934,.T.);
#2437=ORIENTED_EDGE('',*,*,#1932,.T.);
#2438=ORIENTED_EDGE('',*,*,#1934,.F.);
#2439=ORIENTED_EDGE('',*,*,#1924,.T.);
#2440=ORIENTED_EDGE('',*,*,#1894,.F.);
#2441=ORIENTED_EDGE('',*,*,#1912,.F.);
#2442=ORIENTED_EDGE('',*,*,#1901,.T.);
#2443=ORIENTED_EDGE('',*,*,#1898,.T.);
#2444=ORIENTED_EDGE('',*,*,#1935,.T.);
#2445=ORIENTED_EDGE('',*,*,#1904,.F.);
#2446=ORIENTED_EDGE('',*,*,#1936,.F.);
#2447=ORIENTED_EDGE('',*,*,#1905,.F.);
#2448=ORIENTED_EDGE('',*,*,#1935,.F.);
#2449=ORIENTED_EDGE('',*,*,#1897,.T.);
#2450=ORIENTED_EDGE('',*,*,#1937,.F.);
#2451=ORIENTED_EDGE('',*,*,#1916,.T.);
#2452=ORIENTED_EDGE('',*,*,#1938,.F.);
#2453=ORIENTED_EDGE('',*,*,#1920,.F.);
#2454=ORIENTED_EDGE('',*,*,#1939,.F.);
#2455=ORIENTED_EDGE('',*,*,#1922,.T.);
#2456=ORIENTED_EDGE('',*,*,#1940,.F.);
#2457=ORIENTED_EDGE('',*,*,#1914,.F.);
#2458=ORIENTED_EDGE('',*,*,#1941,.F.);
#2459=ORIENTED_EDGE('',*,*,#1908,.F.);
#2460=ORIENTED_EDGE('',*,*,#1942,.F.);
#2461=ORIENTED_EDGE('',*,*,#1928,.T.);
#2462=ORIENTED_EDGE('',*,*,#1943,.F.);
#2463=ORIENTED_EDGE('',*,*,#1910,.T.);
#2464=ORIENTED_EDGE('',*,*,#1944,.F.);
#2465=ORIENTED_EDGE('',*,*,#1926,.F.);
#2466=ORIENTED_EDGE('',*,*,#1945,.F.);
#2467=ORIENTED_EDGE('',*,*,#1930,.T.);
#2468=ORIENTED_EDGE('',*,*,#1892,.T.);
#2469=ORIENTED_EDGE('',*,*,#1917,.T.);
#2470=ORIENTED_EDGE('',*,*,#1939,.T.);
#2471=ORIENTED_EDGE('',*,*,#1937,.T.);
#2472=ORIENTED_EDGE('',*,*,#1896,.T.);
#2473=ORIENTED_EDGE('',*,*,#1923,.T.);
#2474=ORIENTED_EDGE('',*,*,#1941,.T.);
#2475=ORIENTED_EDGE('',*,*,#1913,.T.);
#2476=ORIENTED_EDGE('',*,*,#1899,.T.);
#2477=ORIENTED_EDGE('',*,*,#1921,.T.);
#2478=ORIENTED_EDGE('',*,*,#1938,.T.);
#2479=ORIENTED_EDGE('',*,*,#1915,.T.);
#2480=ORIENTED_EDGE('',*,*,#1940,.T.);
#2481=ORIENTED_EDGE('',*,*,#1925,.T.);
#2482=ORIENTED_EDGE('',*,*,#1906,.T.);
#2483=ORIENTED_EDGE('',*,*,#1936,.T.);
#2484=ORIENTED_EDGE('',*,*,#1903,.T.);
#2485=ORIENTED_EDGE('',*,*,#1911,.T.);
#2486=ORIENTED_EDGE('',*,*,#1945,.T.);
#2487=ORIENTED_EDGE('',*,*,#1927,.T.);
#2488=ORIENTED_EDGE('',*,*,#1944,.T.);
#2489=ORIENTED_EDGE('',*,*,#1909,.T.);
#2490=ORIENTED_EDGE('',*,*,#1943,.T.);
#2491=ORIENTED_EDGE('',*,*,#1929,.T.);
#2492=ORIENTED_EDGE('',*,*,#1942,.T.);
#2493=ORIENTED_EDGE('',*,*,#1907,.T.);
#2494=ORIENTED_EDGE('',*,*,#1890,.T.);
#2495=ORIENTED_EDGE('',*,*,#1946,.T.);
#2496=ORIENTED_EDGE('',*,*,#1947,.T.);
#2497=ORIENTED_EDGE('',*,*,#1948,.F.);
#2498=ORIENTED_EDGE('',*,*,#1949,.T.);
#2499=ORIENTED_EDGE('',*,*,#1950,.F.);
#2500=ORIENTED_EDGE('',*,*,#1951,.T.);
#2501=ORIENTED_EDGE('',*,*,#1952,.T.);
#2502=ORIENTED_EDGE('',*,*,#1953,.T.);
#2503=ORIENTED_EDGE('',*,*,#1954,.T.);
#2504=ORIENTED_EDGE('',*,*,#1955,.T.);
#2505=ORIENTED_EDGE('',*,*,#1956,.F.);
#2506=ORIENTED_EDGE('',*,*,#1957,.F.);
#2507=ORIENTED_EDGE('',*,*,#1958,.T.);
#2508=ORIENTED_EDGE('',*,*,#1959,.F.);
#2509=ORIENTED_EDGE('',*,*,#1960,.F.);
#2510=ORIENTED_EDGE('',*,*,#1961,.T.);
#2511=ORIENTED_EDGE('',*,*,#1962,.T.);
#2512=ORIENTED_EDGE('',*,*,#1963,.T.);
#2513=ORIENTED_EDGE('',*,*,#1948,.T.);
#2514=ORIENTED_EDGE('',*,*,#1964,.T.);
#2515=ORIENTED_EDGE('',*,*,#1965,.T.);
#2516=ORIENTED_EDGE('',*,*,#1966,.T.);
#2517=ORIENTED_EDGE('',*,*,#1967,.F.);
#2518=ORIENTED_EDGE('',*,*,#1968,.T.);
#2519=ORIENTED_EDGE('',*,*,#1950,.T.);
#2520=ORIENTED_EDGE('',*,*,#1969,.F.);
#2521=ORIENTED_EDGE('',*,*,#1962,.F.);
#2522=ORIENTED_EDGE('',*,*,#1970,.T.);
#2523=ORIENTED_EDGE('',*,*,#1971,.T.);
#2524=ORIENTED_EDGE('',*,*,#1972,.T.);
#2525=ORIENTED_EDGE('',*,*,#1973,.F.);
#2526=ORIENTED_EDGE('',*,*,#1974,.T.);
#2527=ORIENTED_EDGE('',*,*,#1975,.F.);
#2528=ORIENTED_EDGE('',*,*,#1976,.F.);
#2529=ORIENTED_EDGE('',*,*,#1977,.F.);
#2530=ORIENTED_EDGE('',*,*,#1978,.T.);
#2531=ORIENTED_EDGE('',*,*,#1946,.F.);
#2532=ORIENTED_EDGE('',*,*,#1979,.T.);
#2533=ORIENTED_EDGE('',*,*,#1980,.T.);
#2534=ORIENTED_EDGE('',*,*,#1981,.T.);
#2535=ORIENTED_EDGE('',*,*,#1982,.F.);
#2536=ORIENTED_EDGE('',*,*,#1983,.T.);
#2537=ORIENTED_EDGE('',*,*,#1957,.T.);
#2538=ORIENTED_EDGE('',*,*,#1984,.T.);
#2539=ORIENTED_EDGE('',*,*,#1955,.F.);
#2540=ORIENTED_EDGE('',*,*,#1985,.T.);
#2541=ORIENTED_EDGE('',*,*,#1986,.T.);
#2542=ORIENTED_EDGE('',*,*,#1987,.T.);
#2543=ORIENTED_EDGE('',*,*,#1988,.T.);
#2544=ORIENTED_EDGE('',*,*,#1989,.T.);
#2545=ORIENTED_EDGE('',*,*,#1975,.T.);
#2546=ORIENTED_EDGE('',*,*,#1990,.T.);
#2547=ORIENTED_EDGE('',*,*,#1988,.F.);
#2548=ORIENTED_EDGE('',*,*,#1990,.F.);
#2549=ORIENTED_EDGE('',*,*,#1976,.T.);
#2550=ORIENTED_EDGE('',*,*,#1991,.T.);
#2551=ORIENTED_EDGE('',*,*,#1989,.F.);
#2552=ORIENTED_EDGE('',*,*,#1991,.F.);
#2553=ORIENTED_EDGE('',*,*,#1984,.F.);
#2554=ORIENTED_EDGE('',*,*,#1963,.F.);
#2555=ORIENTED_EDGE('',*,*,#1969,.T.);
#2556=ORIENTED_EDGE('',*,*,#1956,.T.);
#2557=ORIENTED_EDGE('',*,*,#1952,.F.);
#2558=ORIENTED_EDGE('',*,*,#1992,.T.);
#2559=ORIENTED_EDGE('',*,*,#1953,.F.);
#2560=ORIENTED_EDGE('',*,*,#1993,.T.);
#2561=ORIENTED_EDGE('',*,*,#1959,.T.);
#2562=ORIENTED_EDGE('',*,*,#1994,.T.);
#2563=ORIENTED_EDGE('',*,*,#1960,.T.);
#2564=ORIENTED_EDGE('',*,*,#1993,.F.);
#2565=ORIENTED_EDGE('',*,*,#1965,.F.);
#2566=ORIENTED_EDGE('',*,*,#1995,.T.);
#2567=ORIENTED_EDGE('',*,*,#1977,.T.);
#2568=ORIENTED_EDGE('',*,*,#1996,.T.);
#2569=ORIENTED_EDGE('',*,*,#1986,.F.);
#2570=ORIENTED_EDGE('',*,*,#1997,.T.);
#2571=ORIENTED_EDGE('',*,*,#1967,.T.);
#2572=ORIENTED_EDGE('',*,*,#1998,.T.);
#2573=ORIENTED_EDGE('',*,*,#1973,.T.);
#2574=ORIENTED_EDGE('',*,*,#1999,.T.);
#2575=ORIENTED_EDGE('',*,*,#1980,.F.);
#2576=ORIENTED_EDGE('',*,*,#2000,.T.);
#2577=ORIENTED_EDGE('',*,*,#1971,.F.);
#2578=ORIENTED_EDGE('',*,*,#2001,.T.);
#2579=ORIENTED_EDGE('',*,*,#1982,.T.);
#2580=ORIENTED_EDGE('',*,*,#2002,.T.);
#2581=ORIENTED_EDGE('',*,*,#1978,.F.);
#2582=ORIENTED_EDGE('',*,*,#1995,.F.);
#2583=ORIENTED_EDGE('',*,*,#1964,.F.);
#2584=ORIENTED_EDGE('',*,*,#1947,.F.);
#2585=ORIENTED_EDGE('',*,*,#1992,.F.);
#2586=ORIENTED_EDGE('',*,*,#1951,.F.);
#2587=ORIENTED_EDGE('',*,*,#1968,.F.);
#2588=ORIENTED_EDGE('',*,*,#1997,.F.);
#2589=ORIENTED_EDGE('',*,*,#1985,.F.);
#2590=ORIENTED_EDGE('',*,*,#1954,.F.);
#2591=ORIENTED_EDGE('',*,*,#1987,.F.);
#2592=ORIENTED_EDGE('',*,*,#1998,.F.);
#2593=ORIENTED_EDGE('',*,*,#1966,.F.);
#2594=ORIENTED_EDGE('',*,*,#1996,.F.);
#2595=ORIENTED_EDGE('',*,*,#1983,.F.);
#2596=ORIENTED_EDGE('',*,*,#2001,.F.);
#2597=ORIENTED_EDGE('',*,*,#1970,.F.);
#2598=ORIENTED_EDGE('',*,*,#1961,.F.);
#2599=ORIENTED_EDGE('',*,*,#1994,.F.);
#2600=ORIENTED_EDGE('',*,*,#1958,.F.);
#2601=ORIENTED_EDGE('',*,*,#1981,.F.);
#2602=ORIENTED_EDGE('',*,*,#1999,.F.);
#2603=ORIENTED_EDGE('',*,*,#1972,.F.);
#2604=ORIENTED_EDGE('',*,*,#2002,.F.);
#2605=ORIENTED_EDGE('',*,*,#1979,.F.);
#2606=ORIENTED_EDGE('',*,*,#1949,.F.);
#2607=ORIENTED_EDGE('',*,*,#1974,.F.);
#2608=ORIENTED_EDGE('',*,*,#2000,.F.);
#2609=ORIENTED_EDGE('',*,*,#2003,.T.);
#2610=ORIENTED_EDGE('',*,*,#2004,.T.);
#2611=ORIENTED_EDGE('',*,*,#2005,.F.);
#2612=ORIENTED_EDGE('',*,*,#2006,.T.);
#2613=ORIENTED_EDGE('',*,*,#2007,.F.);
#2614=ORIENTED_EDGE('',*,*,#2008,.T.);
#2615=ORIENTED_EDGE('',*,*,#2009,.T.);
#2616=ORIENTED_EDGE('',*,*,#2010,.T.);
#2617=ORIENTED_EDGE('',*,*,#2011,.T.);
#2618=ORIENTED_EDGE('',*,*,#2012,.T.);
#2619=ORIENTED_EDGE('',*,*,#2013,.F.);
#2620=ORIENTED_EDGE('',*,*,#2014,.F.);
#2621=ORIENTED_EDGE('',*,*,#2015,.T.);
#2622=ORIENTED_EDGE('',*,*,#2016,.F.);
#2623=ORIENTED_EDGE('',*,*,#2017,.F.);
#2624=ORIENTED_EDGE('',*,*,#2018,.T.);
#2625=ORIENTED_EDGE('',*,*,#2019,.T.);
#2626=ORIENTED_EDGE('',*,*,#2020,.T.);
#2627=ORIENTED_EDGE('',*,*,#2005,.T.);
#2628=ORIENTED_EDGE('',*,*,#2021,.T.);
#2629=ORIENTED_EDGE('',*,*,#2022,.T.);
#2630=ORIENTED_EDGE('',*,*,#2023,.T.);
#2631=ORIENTED_EDGE('',*,*,#2024,.F.);
#2632=ORIENTED_EDGE('',*,*,#2025,.T.);
#2633=ORIENTED_EDGE('',*,*,#2007,.T.);
#2634=ORIENTED_EDGE('',*,*,#2026,.F.);
#2635=ORIENTED_EDGE('',*,*,#2019,.F.);
#2636=ORIENTED_EDGE('',*,*,#2027,.T.);
#2637=ORIENTED_EDGE('',*,*,#2028,.T.);
#2638=ORIENTED_EDGE('',*,*,#2029,.T.);
#2639=ORIENTED_EDGE('',*,*,#2030,.F.);
#2640=ORIENTED_EDGE('',*,*,#2031,.T.);
#2641=ORIENTED_EDGE('',*,*,#2032,.F.);
#2642=ORIENTED_EDGE('',*,*,#2033,.F.);
#2643=ORIENTED_EDGE('',*,*,#2034,.F.);
#2644=ORIENTED_EDGE('',*,*,#2035,.T.);
#2645=ORIENTED_EDGE('',*,*,#2003,.F.);
#2646=ORIENTED_EDGE('',*,*,#2036,.T.);
#2647=ORIENTED_EDGE('',*,*,#2037,.T.);
#2648=ORIENTED_EDGE('',*,*,#2038,.T.);
#2649=ORIENTED_EDGE('',*,*,#2039,.F.);
#2650=ORIENTED_EDGE('',*,*,#2040,.T.);
#2651=ORIENTED_EDGE('',*,*,#2014,.T.);
#2652=ORIENTED_EDGE('',*,*,#2041,.T.);
#2653=ORIENTED_EDGE('',*,*,#2012,.F.);
#2654=ORIENTED_EDGE('',*,*,#2042,.T.);
#2655=ORIENTED_EDGE('',*,*,#2043,.T.);
#2656=ORIENTED_EDGE('',*,*,#2044,.T.);
#2657=ORIENTED_EDGE('',*,*,#2045,.T.);
#2658=ORIENTED_EDGE('',*,*,#2046,.T.);
#2659=ORIENTED_EDGE('',*,*,#2032,.T.);
#2660=ORIENTED_EDGE('',*,*,#2047,.T.);
#2661=ORIENTED_EDGE('',*,*,#2045,.F.);
#2662=ORIENTED_EDGE('',*,*,#2047,.F.);
#2663=ORIENTED_EDGE('',*,*,#2033,.T.);
#2664=ORIENTED_EDGE('',*,*,#2048,.T.);
#2665=ORIENTED_EDGE('',*,*,#2046,.F.);
#2666=ORIENTED_EDGE('',*,*,#2048,.F.);
#2667=ORIENTED_EDGE('',*,*,#2041,.F.);
#2668=ORIENTED_EDGE('',*,*,#2020,.F.);
#2669=ORIENTED_EDGE('',*,*,#2026,.T.);
#2670=ORIENTED_EDGE('',*,*,#2013,.T.);
#2671=ORIENTED_EDGE('',*,*,#2009,.F.);
#2672=ORIENTED_EDGE('',*,*,#2049,.T.);
#2673=ORIENTED_EDGE('',*,*,#2010,.F.);
#2674=ORIENTED_EDGE('',*,*,#2050,.T.);
#2675=ORIENTED_EDGE('',*,*,#2016,.T.);
#2676=ORIENTED_EDGE('',*,*,#2051,.T.);
#2677=ORIENTED_EDGE('',*,*,#2017,.T.);
#2678=ORIENTED_EDGE('',*,*,#2050,.F.);
#2679=ORIENTED_EDGE('',*,*,#2022,.F.);
#2680=ORIENTED_EDGE('',*,*,#2052,.T.);
#2681=ORIENTED_EDGE('',*,*,#2034,.T.);
#2682=ORIENTED_EDGE('',*,*,#2053,.T.);
#2683=ORIENTED_EDGE('',*,*,#2043,.F.);
#2684=ORIENTED_EDGE('',*,*,#2054,.T.);
#2685=ORIENTED_EDGE('',*,*,#2024,.T.);
#2686=ORIENTED_EDGE('',*,*,#2055,.T.);
#2687=ORIENTED_EDGE('',*,*,#2030,.T.);
#2688=ORIENTED_EDGE('',*,*,#2056,.T.);
#2689=ORIENTED_EDGE('',*,*,#2037,.F.);
#2690=ORIENTED_EDGE('',*,*,#2057,.T.);
#2691=ORIENTED_EDGE('',*,*,#2028,.F.);
#2692=ORIENTED_EDGE('',*,*,#2058,.T.);
#2693=ORIENTED_EDGE('',*,*,#2039,.T.);
#2694=ORIENTED_EDGE('',*,*,#2059,.T.);
#2695=ORIENTED_EDGE('',*,*,#2035,.F.);
#2696=ORIENTED_EDGE('',*,*,#2052,.F.);
#2697=ORIENTED_EDGE('',*,*,#2021,.F.);
#2698=ORIENTED_EDGE('',*,*,#2004,.F.);
#2699=ORIENTED_EDGE('',*,*,#2049,.F.);
#2700=ORIENTED_EDGE('',*,*,#2008,.F.);
#2701=ORIENTED_EDGE('',*,*,#2025,.F.);
#2702=ORIENTED_EDGE('',*,*,#2054,.F.);
#2703=ORIENTED_EDGE('',*,*,#2042,.F.);
#2704=ORIENTED_EDGE('',*,*,#2011,.F.);
#2705=ORIENTED_EDGE('',*,*,#2044,.F.);
#2706=ORIENTED_EDGE('',*,*,#2055,.F.);
#2707=ORIENTED_EDGE('',*,*,#2023,.F.);
#2708=ORIENTED_EDGE('',*,*,#2053,.F.);
#2709=ORIENTED_EDGE('',*,*,#2040,.F.);
#2710=ORIENTED_EDGE('',*,*,#2058,.F.);
#2711=ORIENTED_EDGE('',*,*,#2027,.F.);
#2712=ORIENTED_EDGE('',*,*,#2018,.F.);
#2713=ORIENTED_EDGE('',*,*,#2051,.F.);
#2714=ORIENTED_EDGE('',*,*,#2015,.F.);
#2715=ORIENTED_EDGE('',*,*,#2038,.F.);
#2716=ORIENTED_EDGE('',*,*,#2056,.F.);
#2717=ORIENTED_EDGE('',*,*,#2029,.F.);
#2718=ORIENTED_EDGE('',*,*,#2059,.F.);
#2719=ORIENTED_EDGE('',*,*,#2036,.F.);
#2720=ORIENTED_EDGE('',*,*,#2006,.F.);
#2721=ORIENTED_EDGE('',*,*,#2031,.F.);
#2722=ORIENTED_EDGE('',*,*,#2057,.F.);
#2723=ORIENTED_EDGE('',*,*,#2060,.T.);
#2724=ORIENTED_EDGE('',*,*,#2061,.F.);
#2725=ORIENTED_EDGE('',*,*,#2062,.F.);
#2726=ORIENTED_EDGE('',*,*,#2063,.F.);
#2727=ORIENTED_EDGE('',*,*,#2064,.F.);
#2728=ORIENTED_EDGE('',*,*,#2065,.F.);
#2729=ORIENTED_EDGE('',*,*,#2066,.T.);
#2730=ORIENTED_EDGE('',*,*,#2067,.F.);
#2731=ORIENTED_EDGE('',*,*,#2068,.T.);
#2732=ORIENTED_EDGE('',*,*,#2069,.F.);
#2733=ORIENTED_EDGE('',*,*,#2070,.F.);
#2734=ORIENTED_EDGE('',*,*,#2071,.F.);
#2735=ORIENTED_EDGE('',*,*,#2072,.F.);
#2736=ORIENTED_EDGE('',*,*,#2073,.F.);
#2737=ORIENTED_EDGE('',*,*,#2074,.T.);
#2738=ORIENTED_EDGE('',*,*,#2075,.F.);
#2739=ORIENTED_EDGE('',*,*,#2076,.F.);
#2740=ORIENTED_EDGE('',*,*,#2077,.F.);
#2741=ORIENTED_EDGE('',*,*,#2078,.F.);
#2742=ORIENTED_EDGE('',*,*,#2079,.T.);
#2743=ORIENTED_EDGE('',*,*,#2080,.T.);
#2744=ORIENTED_EDGE('',*,*,#2079,.F.);
#2745=ORIENTED_EDGE('',*,*,#2081,.F.);
#2746=ORIENTED_EDGE('',*,*,#2082,.F.);
#2747=ORIENTED_EDGE('',*,*,#2083,.T.);
#2748=ORIENTED_EDGE('',*,*,#2084,.F.);
#2749=ORIENTED_EDGE('',*,*,#2085,.F.);
#2750=ORIENTED_EDGE('',*,*,#2086,.T.);
#2751=ORIENTED_EDGE('',*,*,#2087,.T.);
#2752=ORIENTED_EDGE('',*,*,#2086,.F.);
#2753=ORIENTED_EDGE('',*,*,#2088,.F.);
#2754=ORIENTED_EDGE('',*,*,#2089,.F.);
#2755=ORIENTED_EDGE('',*,*,#2090,.F.);
#2756=ORIENTED_EDGE('',*,*,#2083,.F.);
#2757=ORIENTED_EDGE('',*,*,#2091,.F.);
#2758=ORIENTED_EDGE('',*,*,#2066,.F.);
#2759=ORIENTED_EDGE('',*,*,#2092,.F.);
#2760=ORIENTED_EDGE('',*,*,#2070,.T.);
#2761=ORIENTED_EDGE('',*,*,#2093,.F.);
#2762=ORIENTED_EDGE('',*,*,#2076,.T.);
#2763=ORIENTED_EDGE('',*,*,#2094,.F.);
#2764=ORIENTED_EDGE('',*,*,#2060,.F.);
#2765=ORIENTED_EDGE('',*,*,#2095,.F.);
#2766=ORIENTED_EDGE('',*,*,#2096,.F.);
#2767=ORIENTED_EDGE('',*,*,#2080,.F.);
#2768=ORIENTED_EDGE('',*,*,#2087,.F.);
#2769=ORIENTED_EDGE('',*,*,#2085,.T.);
#2770=ORIENTED_EDGE('',*,*,#2078,.T.);
#2771=ORIENTED_EDGE('',*,*,#2062,.T.);
#2772=ORIENTED_EDGE('',*,*,#2097,.F.);
#2773=ORIENTED_EDGE('',*,*,#2074,.F.);
#2774=ORIENTED_EDGE('',*,*,#2098,.F.);
#2775=ORIENTED_EDGE('',*,*,#2068,.F.);
#2776=ORIENTED_EDGE('',*,*,#2099,.F.);
#2777=ORIENTED_EDGE('',*,*,#2064,.T.);
#2778=ORIENTED_EDGE('',*,*,#2100,.F.);
#2779=ORIENTED_EDGE('',*,*,#2081,.T.);
#2780=ORIENTED_EDGE('',*,*,#2101,.F.);
#2781=ORIENTED_EDGE('',*,*,#2102,.F.);
#2782=ORIENTED_EDGE('',*,*,#2103,.T.);
#2783=ORIENTED_EDGE('',*,*,#2104,.F.);
#2784=ORIENTED_EDGE('',*,*,#2105,.F.);
#2785=ORIENTED_EDGE('',*,*,#2100,.T.);
#2786=ORIENTED_EDGE('',*,*,#2067,.T.);
#2787=ORIENTED_EDGE('',*,*,#2091,.T.);
#2788=ORIENTED_EDGE('',*,*,#2082,.T.);
#2789=ORIENTED_EDGE('',*,*,#2099,.T.);
#2790=ORIENTED_EDGE('',*,*,#2071,.T.);
#2791=ORIENTED_EDGE('',*,*,#2092,.T.);
#2792=ORIENTED_EDGE('',*,*,#2065,.T.);
#2793=ORIENTED_EDGE('',*,*,#2098,.T.);
#2794=ORIENTED_EDGE('',*,*,#2077,.T.);
#2795=ORIENTED_EDGE('',*,*,#2093,.T.);
#2796=ORIENTED_EDGE('',*,*,#2069,.T.);
#2797=ORIENTED_EDGE('',*,*,#2097,.T.);
#2798=ORIENTED_EDGE('',*,*,#2061,.T.);
#2799=ORIENTED_EDGE('',*,*,#2094,.T.);
#2800=ORIENTED_EDGE('',*,*,#2075,.T.);
#2801=ORIENTED_EDGE('',*,*,#2103,.F.);
#2802=ORIENTED_EDGE('',*,*,#2106,.F.);
#2803=ORIENTED_EDGE('',*,*,#2107,.T.);
#2804=ORIENTED_EDGE('',*,*,#2108,.F.);
#2805=ORIENTED_EDGE('',*,*,#2088,.T.);
#2806=ORIENTED_EDGE('',*,*,#2109,.F.);
#2807=ORIENTED_EDGE('',*,*,#2110,.T.);
#2808=ORIENTED_EDGE('',*,*,#2111,.T.);
#2809=ORIENTED_EDGE('',*,*,#2112,.F.);
#2810=ORIENTED_EDGE('',*,*,#2073,.T.);
#2811=ORIENTED_EDGE('',*,*,#2113,.T.);
#2812=ORIENTED_EDGE('',*,*,#2114,.F.);
#2813=ORIENTED_EDGE('',*,*,#2107,.F.);
#2814=ORIENTED_EDGE('',*,*,#2115,.F.);
#2815=ORIENTED_EDGE('',*,*,#2113,.F.);
#2816=ORIENTED_EDGE('',*,*,#2072,.T.);
#2817=ORIENTED_EDGE('',*,*,#2116,.T.);
#2818=ORIENTED_EDGE('',*,*,#2110,.F.);
#2819=ORIENTED_EDGE('',*,*,#2117,.F.);
#2820=ORIENTED_EDGE('',*,*,#2111,.F.);
#2821=ORIENTED_EDGE('',*,*,#2116,.F.);
#2822=ORIENTED_EDGE('',*,*,#2112,.T.);
#2823=ORIENTED_EDGE('',*,*,#2117,.T.);
#2824=ORIENTED_EDGE('',*,*,#2109,.T.);
#2825=ORIENTED_EDGE('',*,*,#2096,.T.);
#2826=ORIENTED_EDGE('',*,*,#2118,.T.);
#2827=ORIENTED_EDGE('',*,*,#2104,.T.);
#2828=ORIENTED_EDGE('',*,*,#2105,.T.);
#2829=ORIENTED_EDGE('',*,*,#2118,.F.);
#2830=ORIENTED_EDGE('',*,*,#2095,.T.);
#2831=ORIENTED_EDGE('',*,*,#2063,.T.);
#2832=ORIENTED_EDGE('',*,*,#2119,.T.);
#2833=ORIENTED_EDGE('',*,*,#2089,.T.);
#2834=ORIENTED_EDGE('',*,*,#2108,.T.);
#2835=ORIENTED_EDGE('',*,*,#2114,.T.);
#2836=ORIENTED_EDGE('',*,*,#2115,.T.);
#2837=ORIENTED_EDGE('',*,*,#2106,.T.);
#2838=ORIENTED_EDGE('',*,*,#2102,.T.);
#2839=ORIENTED_EDGE('',*,*,#2101,.T.);
#2840=ORIENTED_EDGE('',*,*,#2084,.T.);
#2841=ORIENTED_EDGE('',*,*,#2090,.T.);
#2842=ORIENTED_EDGE('',*,*,#2119,.F.);
#2843=ORIENTED_EDGE('',*,*,#2120,.F.);
#2844=ORIENTED_EDGE('',*,*,#2121,.T.);
#2845=ORIENTED_EDGE('',*,*,#2122,.T.);
#2846=ORIENTED_EDGE('',*,*,#2123,.T.);
#2847=ORIENTED_EDGE('',*,*,#2124,.T.);
#2848=ORIENTED_EDGE('',*,*,#2125,.T.);
#2849=ORIENTED_EDGE('',*,*,#2126,.F.);
#2850=ORIENTED_EDGE('',*,*,#2127,.T.);
#2851=ORIENTED_EDGE('',*,*,#2128,.F.);
#2852=ORIENTED_EDGE('',*,*,#2129,.T.);
#2853=ORIENTED_EDGE('',*,*,#2130,.T.);
#2854=ORIENTED_EDGE('',*,*,#2131,.T.);
#2855=ORIENTED_EDGE('',*,*,#2132,.T.);
#2856=ORIENTED_EDGE('',*,*,#2133,.T.);
#2857=ORIENTED_EDGE('',*,*,#2134,.F.);
#2858=ORIENTED_EDGE('',*,*,#2135,.T.);
#2859=ORIENTED_EDGE('',*,*,#2136,.T.);
#2860=ORIENTED_EDGE('',*,*,#2137,.T.);
#2861=ORIENTED_EDGE('',*,*,#2138,.T.);
#2862=ORIENTED_EDGE('',*,*,#2139,.T.);
#2863=ORIENTED_EDGE('',*,*,#2140,.F.);
#2864=ORIENTED_EDGE('',*,*,#2139,.F.);
#2865=ORIENTED_EDGE('',*,*,#2141,.T.);
#2866=ORIENTED_EDGE('',*,*,#2142,.T.);
#2867=ORIENTED_EDGE('',*,*,#2143,.F.);
#2868=ORIENTED_EDGE('',*,*,#2144,.T.);
#2869=ORIENTED_EDGE('',*,*,#2145,.T.);
#2870=ORIENTED_EDGE('',*,*,#2146,.T.);
#2871=ORIENTED_EDGE('',*,*,#2147,.F.);
#2872=ORIENTED_EDGE('',*,*,#2146,.F.);
#2873=ORIENTED_EDGE('',*,*,#2148,.T.);
#2874=ORIENTED_EDGE('',*,*,#2149,.T.);
#2875=ORIENTED_EDGE('',*,*,#2150,.T.);
#2876=ORIENTED_EDGE('',*,*,#2120,.T.);
#2877=ORIENTED_EDGE('',*,*,#2151,.T.);
#2878=ORIENTED_EDGE('',*,*,#2136,.F.);
#2879=ORIENTED_EDGE('',*,*,#2152,.T.);
#2880=ORIENTED_EDGE('',*,*,#2130,.F.);
#2881=ORIENTED_EDGE('',*,*,#2153,.T.);
#2882=ORIENTED_EDGE('',*,*,#2126,.T.);
#2883=ORIENTED_EDGE('',*,*,#2154,.T.);
#2884=ORIENTED_EDGE('',*,*,#2143,.T.);
#2885=ORIENTED_EDGE('',*,*,#2155,.T.);
#2886=ORIENTED_EDGE('',*,*,#2156,.T.);
#2887=ORIENTED_EDGE('',*,*,#2140,.T.);
#2888=ORIENTED_EDGE('',*,*,#2147,.T.);
#2889=ORIENTED_EDGE('',*,*,#2145,.F.);
#2890=ORIENTED_EDGE('',*,*,#2138,.F.);
#2891=ORIENTED_EDGE('',*,*,#2122,.F.);
#2892=ORIENTED_EDGE('',*,*,#2157,.T.);
#2893=ORIENTED_EDGE('',*,*,#2158,.T.);
#2894=ORIENTED_EDGE('',*,*,#2159,.F.);
#2895=ORIENTED_EDGE('',*,*,#2160,.T.);
#2896=ORIENTED_EDGE('',*,*,#2161,.T.);
#2897=ORIENTED_EDGE('',*,*,#2141,.F.);
#2898=ORIENTED_EDGE('',*,*,#2162,.T.);
#2899=ORIENTED_EDGE('',*,*,#2124,.F.);
#2900=ORIENTED_EDGE('',*,*,#2163,.T.);
#2901=ORIENTED_EDGE('',*,*,#2128,.T.);
#2902=ORIENTED_EDGE('',*,*,#2164,.T.);
#2903=ORIENTED_EDGE('',*,*,#2134,.T.);
#2904=ORIENTED_EDGE('',*,*,#2165,.T.);
#2905=ORIENTED_EDGE('',*,*,#2162,.F.);
#2906=ORIENTED_EDGE('',*,*,#2144,.F.);
#2907=ORIENTED_EDGE('',*,*,#2154,.F.);
#2908=ORIENTED_EDGE('',*,*,#2125,.F.);
#2909=ORIENTED_EDGE('',*,*,#2163,.F.);
#2910=ORIENTED_EDGE('',*,*,#2127,.F.);
#2911=ORIENTED_EDGE('',*,*,#2153,.F.);
#2912=ORIENTED_EDGE('',*,*,#2129,.F.);
#2913=ORIENTED_EDGE('',*,*,#2164,.F.);
#2914=ORIENTED_EDGE('',*,*,#2131,.F.);
#2915=ORIENTED_EDGE('',*,*,#2152,.F.);
#2916=ORIENTED_EDGE('',*,*,#2135,.F.);
#2917=ORIENTED_EDGE('',*,*,#2165,.F.);
#2918=ORIENTED_EDGE('',*,*,#2137,.F.);
#2919=ORIENTED_EDGE('',*,*,#2151,.F.);
#2920=ORIENTED_EDGE('',*,*,#2123,.F.);
#2921=ORIENTED_EDGE('',*,*,#2159,.T.);
#2922=ORIENTED_EDGE('',*,*,#2166,.T.);
#2923=ORIENTED_EDGE('',*,*,#2167,.F.);
#2924=ORIENTED_EDGE('',*,*,#2168,.F.);
#2925=ORIENTED_EDGE('',*,*,#2169,.T.);
#2926=ORIENTED_EDGE('',*,*,#2148,.F.);
#2927=ORIENTED_EDGE('',*,*,#2170,.T.);
#2928=ORIENTED_EDGE('',*,*,#2171,.F.);
#2929=ORIENTED_EDGE('',*,*,#2172,.T.);
#2930=ORIENTED_EDGE('',*,*,#2133,.F.);
#2931=ORIENTED_EDGE('',*,*,#2173,.T.);
#2932=ORIENTED_EDGE('',*,*,#2174,.T.);
#2933=ORIENTED_EDGE('',*,*,#2171,.T.);
#2934=ORIENTED_EDGE('',*,*,#2175,.T.);
#2935=ORIENTED_EDGE('',*,*,#2173,.F.);
#2936=ORIENTED_EDGE('',*,*,#2132,.F.);
#2937=ORIENTED_EDGE('',*,*,#2176,.T.);
#2938=ORIENTED_EDGE('',*,*,#2167,.T.);
#2939=ORIENTED_EDGE('',*,*,#2177,.T.);
#2940=ORIENTED_EDGE('',*,*,#2168,.T.);
#2941=ORIENTED_EDGE('',*,*,#2176,.F.);
#2942=ORIENTED_EDGE('',*,*,#2166,.F.);
#2943=ORIENTED_EDGE('',*,*,#2158,.F.);
#2944=ORIENTED_EDGE('',*,*,#2178,.F.);
#2945=ORIENTED_EDGE('',*,*,#2149,.F.);
#2946=ORIENTED_EDGE('',*,*,#2169,.F.);
#2947=ORIENTED_EDGE('',*,*,#2177,.F.);
#2948=ORIENTED_EDGE('',*,*,#2157,.F.);
#2949=ORIENTED_EDGE('',*,*,#2121,.F.);
#2950=ORIENTED_EDGE('',*,*,#2150,.F.);
#2951=ORIENTED_EDGE('',*,*,#2178,.T.);
#2952=ORIENTED_EDGE('',*,*,#2179,.F.);
#2953=ORIENTED_EDGE('',*,*,#2160,.F.);
#2954=ORIENTED_EDGE('',*,*,#2172,.F.);
#2955=ORIENTED_EDGE('',*,*,#2174,.F.);
#2956=ORIENTED_EDGE('',*,*,#2175,.F.);
#2957=ORIENTED_EDGE('',*,*,#2170,.F.);
#2958=ORIENTED_EDGE('',*,*,#2156,.F.);
#2959=ORIENTED_EDGE('',*,*,#2161,.F.);
#2960=ORIENTED_EDGE('',*,*,#2179,.T.);
#2961=ORIENTED_EDGE('',*,*,#2155,.F.);
#2962=ORIENTED_EDGE('',*,*,#2142,.F.);
#2963=ORIENTED_EDGE('',*,*,#2180,.T.);
#2964=ORIENTED_EDGE('',*,*,#2181,.T.);
#2965=ORIENTED_EDGE('',*,*,#2182,.T.);
#2966=ORIENTED_EDGE('',*,*,#2183,.T.);
#2967=ORIENTED_EDGE('',*,*,#2181,.F.);
#2968=ORIENTED_EDGE('',*,*,#2184,.T.);
#2969=ORIENTED_EDGE('',*,*,#2185,.T.);
#2970=ORIENTED_EDGE('',*,*,#2186,.T.);
#2971=ORIENTED_EDGE('',*,*,#2180,.F.);
#2972=ORIENTED_EDGE('',*,*,#2187,.T.);
#2973=ORIENTED_EDGE('',*,*,#2186,.F.);
#2974=ORIENTED_EDGE('',*,*,#2187,.F.);
#2975=ORIENTED_EDGE('',*,*,#2184,.F.);
#2976=ORIENTED_EDGE('',*,*,#2185,.F.);
#2977=ORIENTED_EDGE('',*,*,#2188,.T.);
#2978=ORIENTED_EDGE('',*,*,#2182,.F.);
#2979=ORIENTED_EDGE('',*,*,#2183,.F.);
#2980=ORIENTED_EDGE('',*,*,#2188,.F.);
#2981=ORIENTED_EDGE('',*,*,#2189,.T.);
#2982=ORIENTED_EDGE('',*,*,#2190,.T.);
#2983=ORIENTED_EDGE('',*,*,#2191,.T.);
#2984=ORIENTED_EDGE('',*,*,#2190,.F.);
#2985=ORIENTED_EDGE('',*,*,#2192,.T.);
#2986=ORIENTED_EDGE('',*,*,#2193,.F.);
#2987=ORIENTED_EDGE('',*,*,#2191,.F.);
#2988=ORIENTED_EDGE('',*,*,#2189,.F.);
#2989=ORIENTED_EDGE('',*,*,#2194,.T.);
#2990=ORIENTED_EDGE('',*,*,#2195,.T.);
#2991=ORIENTED_EDGE('',*,*,#2194,.F.);
#2992=ORIENTED_EDGE('',*,*,#2192,.F.);
#2993=ORIENTED_EDGE('',*,*,#2196,.T.);
#2994=ORIENTED_EDGE('',*,*,#2197,.T.);
#2995=ORIENTED_EDGE('',*,*,#2193,.T.);
#2996=ORIENTED_EDGE('',*,*,#2197,.F.);
#2997=ORIENTED_EDGE('',*,*,#2198,.T.);
#2998=ORIENTED_EDGE('',*,*,#2199,.F.);
#2999=ORIENTED_EDGE('',*,*,#2200,.T.);
#3000=ORIENTED_EDGE('',*,*,#2198,.F.);
#3001=ORIENTED_EDGE('',*,*,#2196,.F.);
#3002=ORIENTED_EDGE('',*,*,#2200,.F.);
#3003=ORIENTED_EDGE('',*,*,#2201,.T.);
#3004=ORIENTED_EDGE('',*,*,#2202,.T.);
#3005=ORIENTED_EDGE('',*,*,#2203,.T.);
#3006=ORIENTED_EDGE('',*,*,#2202,.F.);
#3007=ORIENTED_EDGE('',*,*,#2204,.T.);
#3008=ORIENTED_EDGE('',*,*,#2205,.F.);
#3009=ORIENTED_EDGE('',*,*,#2203,.F.);
#3010=ORIENTED_EDGE('',*,*,#2206,.F.);
#3011=ORIENTED_EDGE('',*,*,#2207,.T.);
#3012=ORIENTED_EDGE('',*,*,#2204,.F.);
#3013=ORIENTED_EDGE('',*,*,#2201,.F.);
#3014=ORIENTED_EDGE('',*,*,#2207,.F.);
#3015=ORIENTED_EDGE('',*,*,#2208,.T.);
#3016=ORIENTED_EDGE('',*,*,#2209,.T.);
#3017=ORIENTED_EDGE('',*,*,#2205,.T.);
#3018=ORIENTED_EDGE('',*,*,#2209,.F.);
#3019=ORIENTED_EDGE('',*,*,#2210,.T.);
#3020=ORIENTED_EDGE('',*,*,#2208,.F.);
#3021=ORIENTED_EDGE('',*,*,#2211,.T.);
#3022=ORIENTED_EDGE('',*,*,#2212,.T.);
#3023=ORIENTED_EDGE('',*,*,#2211,.F.);
#3024=ORIENTED_EDGE('',*,*,#2210,.F.);
#3025=ORIENTED_EDGE('',*,*,#2213,.F.);
#3026=ORIENTED_EDGE('',*,*,#2206,.T.);
#3027=ORIENTED_EDGE('',*,*,#2214,.F.);
#3028=ORIENTED_EDGE('',*,*,#2215,.T.);
#3029=ORIENTED_EDGE('',*,*,#2213,.T.);
#3030=ORIENTED_EDGE('',*,*,#2215,.F.);
#3031=ORIENTED_EDGE('',*,*,#2214,.T.);
#3032=ORIENTED_EDGE('',*,*,#2216,.F.);
#3033=ORIENTED_EDGE('',*,*,#2217,.F.);
#3034=ORIENTED_EDGE('',*,*,#2218,.T.);
#3035=ORIENTED_EDGE('',*,*,#2216,.T.);
#3036=ORIENTED_EDGE('',*,*,#2218,.F.);
#3037=ORIENTED_EDGE('',*,*,#2219,.F.);
#3038=ORIENTED_EDGE('',*,*,#2220,.T.);
#3039=ORIENTED_EDGE('',*,*,#2217,.T.);
#3040=ORIENTED_EDGE('',*,*,#2220,.F.);
#3041=ORIENTED_EDGE('',*,*,#2221,.F.);
#3042=ORIENTED_EDGE('',*,*,#2222,.T.);
#3043=ORIENTED_EDGE('',*,*,#2219,.T.);
#3044=ORIENTED_EDGE('',*,*,#2222,.F.);
#3045=ORIENTED_EDGE('',*,*,#2221,.T.);
#3046=ORIENTED_EDGE('',*,*,#2223,.T.);
#3047=ORIENTED_EDGE('',*,*,#2224,.F.);
#3048=ORIENTED_EDGE('',*,*,#2223,.F.);
#3049=ORIENTED_EDGE('',*,*,#2225,.F.);
#3050=ORIENTED_EDGE('',*,*,#2226,.T.);
#3051=ORIENTED_EDGE('',*,*,#2224,.T.);
#3052=ORIENTED_EDGE('',*,*,#2226,.F.);
#3053=ORIENTED_EDGE('',*,*,#2227,.F.);
#3054=ORIENTED_EDGE('',*,*,#2225,.T.);
#3055=ORIENTED_EDGE('',*,*,#2228,.F.);
#3056=ORIENTED_EDGE('',*,*,#2229,.T.);
#3057=ORIENTED_EDGE('',*,*,#2227,.T.);
#3058=ORIENTED_EDGE('',*,*,#2229,.F.);
#3059=ORIENTED_EDGE('',*,*,#2228,.T.);
#3060=ORIENTED_EDGE('',*,*,#2195,.F.);
#3061=ORIENTED_EDGE('',*,*,#2199,.T.);
#3062=ORIENTED_EDGE('',*,*,#2230,.F.);
#3063=ORIENTED_EDGE('',*,*,#2231,.F.);
#3064=ORIENTED_EDGE('',*,*,#2232,.T.);
#3065=ORIENTED_EDGE('',*,*,#2230,.T.);
#3066=ORIENTED_EDGE('',*,*,#2232,.F.);
#3067=ORIENTED_EDGE('',*,*,#2233,.F.);
#3068=ORIENTED_EDGE('',*,*,#2231,.T.);
#3069=ORIENTED_EDGE('',*,*,#2234,.F.);
#3070=ORIENTED_EDGE('',*,*,#2235,.T.);
#3071=ORIENTED_EDGE('',*,*,#2233,.T.);
#3072=ORIENTED_EDGE('',*,*,#2235,.F.);
#3073=ORIENTED_EDGE('',*,*,#2234,.T.);
#3074=ORIENTED_EDGE('',*,*,#2236,.F.);
#3075=ORIENTED_EDGE('',*,*,#2237,.F.);
#3076=ORIENTED_EDGE('',*,*,#2238,.T.);
#3077=ORIENTED_EDGE('',*,*,#2236,.T.);
#3078=ORIENTED_EDGE('',*,*,#2238,.F.);
#3079=ORIENTED_EDGE('',*,*,#2212,.F.);
#3080=ORIENTED_EDGE('',*,*,#2237,.T.);
#3081=ORIENTED_EDGE('',*,*,#2239,.T.);
#3082=ORIENTED_EDGE('',*,*,#2240,.F.);
#3083=ORIENTED_EDGE('',*,*,#2239,.F.);
#3084=ORIENTED_EDGE('',*,*,#2241,.T.);
#3085=ORIENTED_EDGE('',*,*,#2242,.T.);
#3086=ORIENTED_EDGE('',*,*,#2241,.F.);
#3087=ORIENTED_EDGE('',*,*,#2242,.F.);
#3088=ORIENTED_EDGE('',*,*,#2243,.T.);
#3089=ORIENTED_EDGE('',*,*,#2244,.T.);
#3090=ORIENTED_EDGE('',*,*,#2245,.T.);
#3091=ORIENTED_EDGE('',*,*,#2243,.F.);
#3092=ORIENTED_EDGE('',*,*,#2245,.F.);
#3093=ORIENTED_EDGE('',*,*,#2244,.F.);
#3094=ORIENTED_EDGE('',*,*,#2246,.T.);
#3095=ORIENTED_EDGE('',*,*,#2247,.T.);
#3096=ORIENTED_EDGE('',*,*,#2246,.F.);
#3097=ORIENTED_EDGE('',*,*,#2248,.T.);
#3098=ORIENTED_EDGE('',*,*,#2247,.F.);
#3099=ORIENTED_EDGE('',*,*,#2240,.T.);
#3100=ORIENTED_EDGE('',*,*,#2249,.T.);
#3101=ORIENTED_EDGE('',*,*,#2248,.F.);
#3102=ORIENTED_EDGE('',*,*,#2249,.F.);
#3103=ORIENTED_EDGE('',*,*,#2250,.F.);
#3104=ORIENTED_EDGE('',*,*,#2251,.T.);
#3105=ORIENTED_EDGE('',*,*,#2252,.F.);
#3106=ORIENTED_EDGE('',*,*,#2253,.T.);
#3107=ORIENTED_EDGE('',*,*,#2250,.T.);
#3108=ORIENTED_EDGE('',*,*,#2253,.F.);
#3109=ORIENTED_EDGE('',*,*,#2252,.T.);
#3110=ORIENTED_EDGE('',*,*,#2254,.F.);
#3111=ORIENTED_EDGE('',*,*,#2255,.F.);
#3112=ORIENTED_EDGE('',*,*,#2256,.T.);
#3113=ORIENTED_EDGE('',*,*,#2254,.T.);
#3114=ORIENTED_EDGE('',*,*,#2256,.F.);
#3115=ORIENTED_EDGE('',*,*,#2257,.F.);
#3116=ORIENTED_EDGE('',*,*,#2258,.T.);
#3117=ORIENTED_EDGE('',*,*,#2255,.T.);
#3118=ORIENTED_EDGE('',*,*,#2258,.F.);
#3119=ORIENTED_EDGE('',*,*,#2259,.F.);
#3120=ORIENTED_EDGE('',*,*,#2257,.T.);
#3121=ORIENTED_EDGE('',*,*,#2251,.F.);
#3122=ORIENTED_EDGE('',*,*,#2260,.T.);
#3123=ORIENTED_EDGE('',*,*,#2259,.T.);
#3124=ORIENTED_EDGE('',*,*,#2260,.F.);
#3125=ORIENTED_EDGE('',*,*,#2261,.T.);
#3126=ORIENTED_EDGE('',*,*,#2262,.F.);
#3127=ORIENTED_EDGE('',*,*,#2261,.F.);
#3128=ORIENTED_EDGE('',*,*,#2263,.T.);
#3129=ORIENTED_EDGE('',*,*,#2264,.T.);
#3130=ORIENTED_EDGE('',*,*,#2263,.F.);
#3131=ORIENTED_EDGE('',*,*,#2264,.F.);
#3132=ORIENTED_EDGE('',*,*,#2265,.T.);
#3133=ORIENTED_EDGE('',*,*,#2265,.F.);
#3134=ORIENTED_EDGE('',*,*,#2266,.T.);
#3135=ORIENTED_EDGE('',*,*,#2262,.T.);
#3136=ORIENTED_EDGE('',*,*,#2266,.F.);
#3137=PLANE('',#3523);
#3138=PLANE('',#3524);
#3139=PLANE('',#3527);
#3140=PLANE('',#3530);
#3141=PLANE('',#3539);
#3142=PLANE('',#3550);
#3143=PLANE('',#3552);
#3144=PLANE('',#3553);
#3145=PLANE('',#3554);
#3146=PLANE('',#3555);
#3147=PLANE('',#3563);
#3148=PLANE('',#3564);
#3149=PLANE('',#3567);
#3150=PLANE('',#3570);
#3151=PLANE('',#3579);
#3152=PLANE('',#3590);
#3153=PLANE('',#3592);
#3154=PLANE('',#3593);
#3155=PLANE('',#3594);
#3156=PLANE('',#3595);
#3157=PLANE('',#3603);
#3158=PLANE('',#3604);
#3159=PLANE('',#3607);
#3160=PLANE('',#3610);
#3161=PLANE('',#3619);
#3162=PLANE('',#3630);
#3163=PLANE('',#3632);
#3164=PLANE('',#3633);
#3165=PLANE('',#3634);
#3166=PLANE('',#3635);
#3167=PLANE('',#3643);
#3168=PLANE('',#3644);
#3169=PLANE('',#3647);
#3170=PLANE('',#3650);
#3171=PLANE('',#3659);
#3172=PLANE('',#3670);
#3173=PLANE('',#3672);
#3174=PLANE('',#3673);
#3175=PLANE('',#3674);
#3176=PLANE('',#3675);
#3177=PLANE('',#3684);
#3178=PLANE('',#3685);
#3179=PLANE('',#3686);
#3180=PLANE('',#3689);
#3181=PLANE('',#3693);
#3182=PLANE('',#3697);
#3183=PLANE('',#3706);
#3184=PLANE('',#3707);
#3185=PLANE('',#3708);
#3186=PLANE('',#3721);
#3187=PLANE('',#3732);
#3188=PLANE('',#3733);
#3189=PLANE('',#3734);
#3190=PLANE('',#3737);
#3191=PLANE('',#3741);
#3192=PLANE('',#3745);
#3193=PLANE('',#3754);
#3194=PLANE('',#3755);
#3195=PLANE('',#3756);
#3196=PLANE('',#3769);
#3197=PLANE('',#3785);
#3198=PLANE('',#3787);
#3199=PLANE('',#3809);
#3200=PLANE('',#3822);
#3201=PLANE('',#3831);
#3202=PLANE('',#3835);
#3203=PLANE('',#3847);
#3204=PLANE('',#3851);
#3205=PLANE('',#3852);
#3206=PLANE('',#3856);
#3207=PLANE('',#3860);
#3208=PLANE('',#3864);
#3209=PLANE('',#3866);
#3210=PLANE('',#3871);
#3211=PLANE('',#3877);
#3212=PLANE('',#3881);
#3213=PLANE('',#3886);
#3214=PLANE('',#3892);
#3215=PLANE('',#3896);
#3216=PLANE('',#3901);
#3217=ADVANCED_FACE('',(#694),#3137,.F.);
#3218=ADVANCED_FACE('',(#695),#3138,.F.);
#3219=ADVANCED_FACE('',(#696),#3139,.T.);
#3220=ADVANCED_FACE('',(#697,#464,#465),#3140,.T.);
#3221=ADVANCED_FACE('',(#698,#466,#467),#3141,.F.);
#3222=ADVANCED_FACE('',(#699),#385,.F.);
#3223=ADVANCED_FACE('',(#700),#386,.F.);
#3224=ADVANCED_FACE('',(#701),#3142,.T.);
#3225=ADVANCED_FACE('',(#702),#387,.F.);
#3226=ADVANCED_FACE('',(#703),#3143,.T.);
#3227=ADVANCED_FACE('',(#704),#3144,.F.);
#3228=ADVANCED_FACE('',(#705),#3145,.F.);
#3229=ADVANCED_FACE('',(#706),#3146,.T.);
#3230=ADVANCED_FACE('',(#707),#388,.T.);
#3231=ADVANCED_FACE('',(#708),#389,.T.);
#3232=ADVANCED_FACE('',(#709),#390,.F.);
#3233=ADVANCED_FACE('',(#710),#391,.T.);
#3234=ADVANCED_FACE('',(#711),#392,.F.);
#3235=ADVANCED_FACE('',(#712),#393,.T.);
#3236=ADVANCED_FACE('',(#713),#3147,.F.);
#3237=ADVANCED_FACE('',(#714),#3148,.F.);
#3238=ADVANCED_FACE('',(#715),#3149,.T.);
#3239=ADVANCED_FACE('',(#716,#468,#469),#3150,.T.);
#3240=ADVANCED_FACE('',(#717,#470,#471),#3151,.F.);
#3241=ADVANCED_FACE('',(#718),#394,.F.);
#3242=ADVANCED_FACE('',(#719),#395,.F.);
#3243=ADVANCED_FACE('',(#720),#3152,.T.);
#3244=ADVANCED_FACE('',(#721),#396,.F.);
#3245=ADVANCED_FACE('',(#722),#3153,.T.);
#3246=ADVANCED_FACE('',(#723),#3154,.F.);
#3247=ADVANCED_FACE('',(#724),#3155,.F.);
#3248=ADVANCED_FACE('',(#725),#3156,.T.);
#3249=ADVANCED_FACE('',(#726),#397,.T.);
#3250=ADVANCED_FACE('',(#727),#398,.T.);
#3251=ADVANCED_FACE('',(#728),#399,.F.);
#3252=ADVANCED_FACE('',(#729),#400,.T.);
#3253=ADVANCED_FACE('',(#730),#401,.F.);
#3254=ADVANCED_FACE('',(#731),#402,.T.);
#3255=ADVANCED_FACE('',(#732),#3157,.F.);
#3256=ADVANCED_FACE('',(#733),#3158,.F.);
#3257=ADVANCED_FACE('',(#734),#3159,.T.);
#3258=ADVANCED_FACE('',(#735,#472,#473),#3160,.T.);
#3259=ADVANCED_FACE('',(#736,#474,#475),#3161,.F.);
#3260=ADVANCED_FACE('',(#737),#403,.F.);
#3261=ADVANCED_FACE('',(#738),#404,.F.);
#3262=ADVANCED_FACE('',(#739),#3162,.T.);
#3263=ADVANCED_FACE('',(#740),#405,.F.);
#3264=ADVANCED_FACE('',(#741),#3163,.T.);
#3265=ADVANCED_FACE('',(#742),#3164,.F.);
#3266=ADVANCED_FACE('',(#743),#3165,.F.);
#3267=ADVANCED_FACE('',(#744),#3166,.T.);
#3268=ADVANCED_FACE('',(#745),#406,.T.);
#3269=ADVANCED_FACE('',(#746),#407,.T.);
#3270=ADVANCED_FACE('',(#747),#408,.F.);
#3271=ADVANCED_FACE('',(#748),#409,.T.);
#3272=ADVANCED_FACE('',(#749),#410,.F.);
#3273=ADVANCED_FACE('',(#750),#411,.T.);
#3274=ADVANCED_FACE('',(#751),#3167,.F.);
#3275=ADVANCED_FACE('',(#752),#3168,.F.);
#3276=ADVANCED_FACE('',(#753),#3169,.T.);
#3277=ADVANCED_FACE('',(#754,#476,#477),#3170,.T.);
#3278=ADVANCED_FACE('',(#755,#478,#479),#3171,.F.);
#3279=ADVANCED_FACE('',(#756),#412,.F.);
#3280=ADVANCED_FACE('',(#757),#413,.F.);
#3281=ADVANCED_FACE('',(#758),#3172,.T.);
#3282=ADVANCED_FACE('',(#759),#414,.F.);
#3283=ADVANCED_FACE('',(#760),#3173,.T.);
#3284=ADVANCED_FACE('',(#761),#3174,.F.);
#3285=ADVANCED_FACE('',(#762),#3175,.F.);
#3286=ADVANCED_FACE('',(#763),#3176,.T.);
#3287=ADVANCED_FACE('',(#764),#415,.T.);
#3288=ADVANCED_FACE('',(#765),#416,.T.);
#3289=ADVANCED_FACE('',(#766),#417,.F.);
#3290=ADVANCED_FACE('',(#767),#418,.T.);
#3291=ADVANCED_FACE('',(#768),#419,.F.);
#3292=ADVANCED_FACE('',(#769),#420,.T.);
#3293=ADVANCED_FACE('',(#770),#3177,.T.);
#3294=ADVANCED_FACE('',(#771),#3178,.T.);
#3295=ADVANCED_FACE('',(#772,#480,#481),#3179,.F.);
#3296=ADVANCED_FACE('',(#773),#3180,.F.);
#3297=ADVANCED_FACE('',(#774),#421,.F.);
#3298=ADVANCED_FACE('',(#775),#3181,.T.);
#3299=ADVANCED_FACE('',(#776),#422,.F.);
#3300=ADVANCED_FACE('',(#777,#482,#483),#3182,.F.);
#3301=ADVANCED_FACE('',(#778),#3183,.F.);
#3302=ADVANCED_FACE('',(#779),#3184,.F.);
#3303=ADVANCED_FACE('',(#780),#3185,.T.);
#3304=ADVANCED_FACE('',(#781),#423,.T.);
#3305=ADVANCED_FACE('',(#782),#424,.T.);
#3306=ADVANCED_FACE('',(#783),#425,.T.);
#3307=ADVANCED_FACE('',(#784),#426,.T.);
#3308=ADVANCED_FACE('',(#785),#3186,.T.);
#3309=ADVANCED_FACE('',(#786),#427,.F.);
#3310=ADVANCED_FACE('',(#787),#428,.F.);
#3311=ADVANCED_FACE('',(#788),#429,.T.);
#3312=ADVANCED_FACE('',(#789),#430,.F.);
#3313=ADVANCED_FACE('',(#790),#431,.T.);
#3314=ADVANCED_FACE('',(#791),#432,.F.);
#3315=ADVANCED_FACE('',(#792),#3187,.T.);
#3316=ADVANCED_FACE('',(#793),#3188,.T.);
#3317=ADVANCED_FACE('',(#794,#484,#485),#3189,.F.);
#3318=ADVANCED_FACE('',(#795),#3190,.F.);
#3319=ADVANCED_FACE('',(#796),#433,.F.);
#3320=ADVANCED_FACE('',(#797),#3191,.T.);
#3321=ADVANCED_FACE('',(#798),#434,.F.);
#3322=ADVANCED_FACE('',(#799,#486,#487),#3192,.F.);
#3323=ADVANCED_FACE('',(#800),#3193,.F.);
#3324=ADVANCED_FACE('',(#801),#3194,.F.);
#3325=ADVANCED_FACE('',(#802),#3195,.T.);
#3326=ADVANCED_FACE('',(#803),#435,.T.);
#3327=ADVANCED_FACE('',(#804),#436,.T.);
#3328=ADVANCED_FACE('',(#805),#437,.T.);
#3329=ADVANCED_FACE('',(#806),#438,.T.);
#3330=ADVANCED_FACE('',(#807),#3196,.T.);
#3331=ADVANCED_FACE('',(#808),#439,.F.);
#3332=ADVANCED_FACE('',(#809),#440,.F.);
#3333=ADVANCED_FACE('',(#810),#441,.T.);
#3334=ADVANCED_FACE('',(#811),#442,.F.);
#3335=ADVANCED_FACE('',(#812),#443,.T.);
#3336=ADVANCED_FACE('',(#813),#444,.F.);
#3337=ADVANCED_FACE('',(#814),#445,.T.);
#3338=ADVANCED_FACE('',(#815),#3197,.T.);
#3339=ADVANCED_FACE('',(#816),#3198,.F.);
#3340=ADVANCED_FACE('',(#817),#325,.T.);
#3341=ADVANCED_FACE('',(#818),#326,.T.);
#3342=ADVANCED_FACE('',(#819),#315,.F.);
#3343=ADVANCED_FACE('',(#820,#488),#3199,.T.);
#3344=ADVANCED_FACE('',(#821),#446,.F.);
#3345=ADVANCED_FACE('',(#822),#316,.T.);
#3346=ADVANCED_FACE('',(#823),#447,.T.);
#3347=ADVANCED_FACE('',(#824),#317,.F.);
#3348=ADVANCED_FACE('',(#825,#489),#3200,.T.);
#3349=ADVANCED_FACE('',(#826),#448,.F.);
#3350=ADVANCED_FACE('',(#827),#318,.T.);
#3351=ADVANCED_FACE('',(#828),#449,.T.);
#3352=ADVANCED_FACE('',(#829,#490),#3201,.T.);
#3353=ADVANCED_FACE('',(#830),#450,.F.);
#3354=ADVANCED_FACE('',(#831,#491),#3202,.T.);
#3355=ADVANCED_FACE('',(#832),#451,.F.);
#3356=ADVANCED_FACE('',(#833),#319,.F.);
#3357=ADVANCED_FACE('',(#834),#452,.F.);
#3358=ADVANCED_FACE('',(#835),#320,.F.);
#3359=ADVANCED_FACE('',(#836),#453,.F.);
#3360=ADVANCED_FACE('',(#837,#492),#3203,.T.);
#3361=ADVANCED_FACE('',(#838),#454,.F.);
#3362=ADVANCED_FACE('',(#839,#493),#3204,.T.);
#3363=ADVANCED_FACE('',(#840,#494),#3205,.T.);
#3364=ADVANCED_FACE('',(#841),#455,.T.);
#3365=ADVANCED_FACE('',(#842,#495),#3206,.T.);
#3366=ADVANCED_FACE('',(#843),#456,.T.);
#3367=ADVANCED_FACE('',(#844,#496),#3207,.T.);
#3368=ADVANCED_FACE('',(#845),#457,.T.);
#3369=ADVANCED_FACE('',(#846,#497),#3208,.T.);
#3370=ADVANCED_FACE('',(#847,#498),#3209,.F.);
#3371=ADVANCED_FACE('',(#848),#458,.T.);
#3372=ADVANCED_FACE('',(#849,#499),#3210,.F.);
#3373=ADVANCED_FACE('',(#850),#321,.F.);
#3374=ADVANCED_FACE('',(#851),#459,.F.);
#3375=ADVANCED_FACE('',(#852,#500),#3211,.F.);
#3376=ADVANCED_FACE('',(#853),#322,.T.);
#3377=ADVANCED_FACE('',(#854,#501),#3212,.T.);
#3378=ADVANCED_FACE('',(#855),#460,.T.);
#3379=ADVANCED_FACE('',(#856,#502),#3213,.T.);
#3380=ADVANCED_FACE('',(#857),#323,.F.);
#3381=ADVANCED_FACE('',(#858),#461,.F.);
#3382=ADVANCED_FACE('',(#859,#503),#3214,.T.);
#3383=ADVANCED_FACE('',(#860),#324,.T.);
#3384=ADVANCED_FACE('',(#861,#504),#3215,.F.);
#3385=ADVANCED_FACE('',(#862),#462,.T.);
#3386=ADVANCED_FACE('',(#863,#505),#3216,.F.);
#3387=ADVANCED_FACE('',(#864),#463,.F.);
#3388=CLOSED_SHELL('',(#3217,#3218,#3219,#3220,#3221,#3222,#3223,#3224,
#3225,#3226,#3227,#3228,#3229,#3230,#3231,#3232,#3233,#3234,#3235));
#3389=CLOSED_SHELL('',(#3236,#3237,#3238,#3239,#3240,#3241,#3242,#3243,
#3244,#3245,#3246,#3247,#3248,#3249,#3250,#3251,#3252,#3253,#3254));
#3390=CLOSED_SHELL('',(#3255,#3256,#3257,#3258,#3259,#3260,#3261,#3262,
#3263,#3264,#3265,#3266,#3267,#3268,#3269,#3270,#3271,#3272,#3273));
#3391=CLOSED_SHELL('',(#3274,#3275,#3276,#3277,#3278,#3279,#3280,#3281,
#3282,#3283,#3284,#3285,#3286,#3287,#3288,#3289,#3290,#3291,#3292));
#3392=CLOSED_SHELL('',(#3293,#3294,#3295,#3296,#3297,#3298,#3299,#3300,
#3301,#3302,#3303,#3304,#3305,#3306,#3307,#3308,#3309,#3310,#3311,#3312,
#3313,#3314));
#3393=CLOSED_SHELL('',(#3315,#3316,#3317,#3318,#3319,#3320,#3321,#3322,
#3323,#3324,#3325,#3326,#3327,#3328,#3329,#3330,#3331,#3332,#3333,#3334,
#3335,#3336));
#3394=CLOSED_SHELL('',(#3337,#3338,#3339,#3340,#3341));
#3395=CLOSED_SHELL('',(#3342,#3343,#3344,#3345,#3346,#3347,#3348,#3349,
#3350,#3351,#3352,#3353,#3354,#3355,#3356,#3357,#3358,#3359,#3360,#3361,
#3362,#3363,#3364,#3365,#3366,#3367,#3368,#3369));
#3396=CLOSED_SHELL('',(#3370,#3371,#3372,#3373,#3374,#3375,#3376));
#3397=CLOSED_SHELL('',(#3377,#3378,#3379,#3380,#3381,#3382,#3383));
#3398=CLOSED_SHELL('',(#3384,#3385,#3386,#3387));
#3399=DERIVED_UNIT_ELEMENT(#3421,1.);
#3400=DERIVED_UNIT_ELEMENT(#6349,-3.);
#3401=DERIVED_UNIT_ELEMENT(#3421,1.);
#3402=DERIVED_UNIT_ELEMENT(#6349,-3.);
#3403=DERIVED_UNIT_ELEMENT(#3421,1.);
#3404=DERIVED_UNIT_ELEMENT(#6349,-3.);
#3405=DERIVED_UNIT_ELEMENT(#3421,1.);
#3406=DERIVED_UNIT_ELEMENT(#6349,-3.);
#3407=DERIVED_UNIT_ELEMENT(#3421,1.);
#3408=DERIVED_UNIT_ELEMENT(#6349,-3.);
#3409=DERIVED_UNIT_ELEMENT(#3421,1.);
#3410=DERIVED_UNIT_ELEMENT(#6349,-3.);
#3411=DERIVED_UNIT_ELEMENT(#3421,1.);
#3412=DERIVED_UNIT_ELEMENT(#6349,-3.);
#3413=DERIVED_UNIT_ELEMENT(#3421,1.);
#3414=DERIVED_UNIT_ELEMENT(#6349,-3.);
#3415=DERIVED_UNIT_ELEMENT(#3421,1.);
#3416=DERIVED_UNIT_ELEMENT(#6349,-3.);
#3417=DERIVED_UNIT_ELEMENT(#3421,1.);
#3418=DERIVED_UNIT_ELEMENT(#6349,-3.);
#3419=DERIVED_UNIT_ELEMENT(#3421,1.);
#3420=DERIVED_UNIT_ELEMENT(#6349,-3.);
#3421=(
MASS_UNIT()
NAMED_UNIT(*)
SI_UNIT(.KILO.,.GRAM.)
);
#3422=DERIVED_UNIT((#3399,#3400));
#3423=DERIVED_UNIT((#3401,#3402));
#3424=DERIVED_UNIT((#3403,#3404));
#3425=DERIVED_UNIT((#3405,#3406));
#3426=DERIVED_UNIT((#3407,#3408));
#3427=DERIVED_UNIT((#3409,#3410));
#3428=DERIVED_UNIT((#3411,#3412));
#3429=DERIVED_UNIT((#3413,#3414));
#3430=DERIVED_UNIT((#3415,#3416));
#3431=DERIVED_UNIT((#3417,#3418));
#3432=DERIVED_UNIT((#3419,#3420));
#3433=MEASURE_REPRESENTATION_ITEM('density measure',
POSITIVE_RATIO_MEASURE(7850.),#3422);
#3434=MEASURE_REPRESENTATION_ITEM('density measure',
POSITIVE_RATIO_MEASURE(7850.),#3423);
#3435=MEASURE_REPRESENTATION_ITEM('density measure',
POSITIVE_RATIO_MEASURE(7850.),#3424);
#3436=MEASURE_REPRESENTATION_ITEM('density measure',
POSITIVE_RATIO_MEASURE(7850.),#3425);
#3437=MEASURE_REPRESENTATION_ITEM('density measure',
POSITIVE_RATIO_MEASURE(7850.),#3426);
#3438=MEASURE_REPRESENTATION_ITEM('density measure',
POSITIVE_RATIO_MEASURE(7850.),#3427);
#3439=MEASURE_REPRESENTATION_ITEM('density measure',
POSITIVE_RATIO_MEASURE(7850.),#3428);
#3440=MEASURE_REPRESENTATION_ITEM('density measure',
POSITIVE_RATIO_MEASURE(7850.),#3429);
#3441=MEASURE_REPRESENTATION_ITEM('density measure',
POSITIVE_RATIO_MEASURE(7850.),#3430);
#3442=MEASURE_REPRESENTATION_ITEM('density measure',
POSITIVE_RATIO_MEASURE(7850.),#3431);
#3443=MEASURE_REPRESENTATION_ITEM('density measure',
POSITIVE_RATIO_MEASURE(7850.),#3432);
#3444=PROPERTY_DEFINITION_REPRESENTATION(#3499,#3466);
#3445=PROPERTY_DEFINITION_REPRESENTATION(#3500,#3467);
#3446=PROPERTY_DEFINITION_REPRESENTATION(#3501,#3468);
#3447=PROPERTY_DEFINITION_REPRESENTATION(#3502,#3469);
#3448=PROPERTY_DEFINITION_REPRESENTATION(#3503,#3470);
#3449=PROPERTY_DEFINITION_REPRESENTATION(#3504,#3471);
#3450=PROPERTY_DEFINITION_REPRESENTATION(#3505,#3472);
#3451=PROPERTY_DEFINITION_REPRESENTATION(#3506,#3473);
#3452=PROPERTY_DEFINITION_REPRESENTATION(#3507,#3474);
#3453=PROPERTY_DEFINITION_REPRESENTATION(#3508,#3475);
#3454=PROPERTY_DEFINITION_REPRESENTATION(#3509,#3476);
#3455=PROPERTY_DEFINITION_REPRESENTATION(#3510,#3477);
#3456=PROPERTY_DEFINITION_REPRESENTATION(#3511,#3478);
#3457=PROPERTY_DEFINITION_REPRESENTATION(#3512,#3479);
#3458=PROPERTY_DEFINITION_REPRESENTATION(#3513,#3480);
#3459=PROPERTY_DEFINITION_REPRESENTATION(#3514,#3481);
#3460=PROPERTY_DEFINITION_REPRESENTATION(#3515,#3482);
#3461=PROPERTY_DEFINITION_REPRESENTATION(#3516,#3483);
#3462=PROPERTY_DEFINITION_REPRESENTATION(#3517,#3484);
#3463=PROPERTY_DEFINITION_REPRESENTATION(#3518,#3485);
#3464=PROPERTY_DEFINITION_REPRESENTATION(#3519,#3486);
#3465=PROPERTY_DEFINITION_REPRESENTATION(#3520,#3487);
#3466=REPRESENTATION('material name',(#3488),#6325);
#3467=REPRESENTATION('density',(#3433),#6325);
#3468=REPRESENTATION('material name',(#3489),#6326);
#3469=REPRESENTATION('density',(#3434),#6326);
#3470=REPRESENTATION('material name',(#3490),#6327);
#3471=REPRESENTATION('density',(#3435),#6327);
#3472=REPRESENTATION('material name',(#3491),#6328);
#3473=REPRESENTATION('density',(#3436),#6328);
#3474=REPRESENTATION('material name',(#3492),#6330);
#3475=REPRESENTATION('density',(#3437),#6330);
#3476=REPRESENTATION('material name',(#3493),#6331);
#3477=REPRESENTATION('density',(#3438),#6331);
#3478=REPRESENTATION('material name',(#3494),#6332);
#3479=REPRESENTATION('density',(#3439),#6332);
#3480=REPRESENTATION('material name',(#3495),#6344);
#3481=REPRESENTATION('density',(#3440),#6344);
#3482=REPRESENTATION('material name',(#3496),#6345);
#3483=REPRESENTATION('density',(#3441),#6345);
#3484=REPRESENTATION('material name',(#3497),#6346);
#3485=REPRESENTATION('density',(#3442),#6346);
#3486=REPRESENTATION('material name',(#3498),#6347);
#3487=REPRESENTATION('density',(#3443),#6347);
#3488=DESCRIPTIVE_REPRESENTATION_ITEM('Steel','Steel');
#3489=DESCRIPTIVE_REPRESENTATION_ITEM('Steel','Steel');
#3490=DESCRIPTIVE_REPRESENTATION_ITEM('Steel','Steel');
#3491=DESCRIPTIVE_REPRESENTATION_ITEM('Steel','Steel');
#3492=DESCRIPTIVE_REPRESENTATION_ITEM('Steel','Steel');
#3493=DESCRIPTIVE_REPRESENTATION_ITEM('Steel','Steel');
#3494=DESCRIPTIVE_REPRESENTATION_ITEM('Steel','Steel');
#3495=DESCRIPTIVE_REPRESENTATION_ITEM('Steel','Steel');
#3496=DESCRIPTIVE_REPRESENTATION_ITEM('Steel','Steel');
#3497=DESCRIPTIVE_REPRESENTATION_ITEM('Steel','Steel');
#3498=DESCRIPTIVE_REPRESENTATION_ITEM('Steel','Steel');
#3499=PROPERTY_DEFINITION('material property','material name',#6502);
#3500=PROPERTY_DEFINITION('material property','density of part',#6502);
#3501=PROPERTY_DEFINITION('material property','material name',#6503);
#3502=PROPERTY_DEFINITION('material property','density of part',#6503);
#3503=PROPERTY_DEFINITION('material property','material name',#6504);
#3504=PROPERTY_DEFINITION('material property','density of part',#6504);
#3505=PROPERTY_DEFINITION('material property','material name',#6505);
#3506=PROPERTY_DEFINITION('material property','density of part',#6505);
#3507=PROPERTY_DEFINITION('material property','material name',#6507);
#3508=PROPERTY_DEFINITION('material property','density of part',#6507);
#3509=PROPERTY_DEFINITION('material property','material name',#6508);
#3510=PROPERTY_DEFINITION('material property','density of part',#6508);
#3511=PROPERTY_DEFINITION('material property','material name',#6509);
#3512=PROPERTY_DEFINITION('material property','density of part',#6509);
#3513=PROPERTY_DEFINITION('material property','material name',#6521);
#3514=PROPERTY_DEFINITION('material property','density of part',#6521);
#3515=PROPERTY_DEFINITION('material property','material name',#6522);
#3516=PROPERTY_DEFINITION('material property','density of part',#6522);
#3517=PROPERTY_DEFINITION('material property','material name',#6523);
#3518=PROPERTY_DEFINITION('material property','density of part',#6523);
#3519=PROPERTY_DEFINITION('material property','material name',#6524);
#3520=PROPERTY_DEFINITION('material property','density of part',#6524);
#3521=AXIS2_PLACEMENT_3D('',#5131,#3980,#3981);
#3522=AXIS2_PLACEMENT_3D('',#5132,#3982,#3983);
#3523=AXIS2_PLACEMENT_3D('',#5133,#3984,#3985);
#3524=AXIS2_PLACEMENT_3D('',#5142,#3990,#3991);
#3525=AXIS2_PLACEMENT_3D('',#5153,#3996,#3997);
#3526=AXIS2_PLACEMENT_3D('',#5155,#3998,#3999);
#3527=AXIS2_PLACEMENT_3D('',#5157,#4001,#4002);
#3528=AXIS2_PLACEMENT_3D('',#5168,#4007,#4008);
#3529=AXIS2_PLACEMENT_3D('',#5170,#4009,#4010);
#3530=AXIS2_PLACEMENT_3D('',#5172,#4012,#4013);
#3531=AXIS2_PLACEMENT_3D('',#5174,#4014,#4015);
#3532=AXIS2_PLACEMENT_3D('',#5178,#4017,#4018);
#3533=AXIS2_PLACEMENT_3D('',#5181,#4020,#4021);
#3534=AXIS2_PLACEMENT_3D('',#5184,#4023,#4024);
#3535=AXIS2_PLACEMENT_3D('',#5188,#4026,#4027);
#3536=AXIS2_PLACEMENT_3D('',#5191,#4029,#4030);
#3537=AXIS2_PLACEMENT_3D('',#5193,#4031,#4032);
#3538=AXIS2_PLACEMENT_3D('',#5195,#4033,#4034);
#3539=AXIS2_PLACEMENT_3D('',#5196,#4035,#4036);
#3540=AXIS2_PLACEMENT_3D('',#5201,#4038,#4039);
#3541=AXIS2_PLACEMENT_3D('',#5204,#4041,#4042);
#3542=AXIS2_PLACEMENT_3D('',#5207,#4044,#4045);
#3543=AXIS2_PLACEMENT_3D('',#5211,#4047,#4048);
#3544=AXIS2_PLACEMENT_3D('',#5214,#4050,#4051);
#3545=AXIS2_PLACEMENT_3D('',#5215,#4052,#4053);
#3546=AXIS2_PLACEMENT_3D('',#5217,#4054,#4055);
#3547=AXIS2_PLACEMENT_3D('',#5219,#4056,#4057);
#3548=AXIS2_PLACEMENT_3D('',#5220,#4058,#4059);
#3549=AXIS2_PLACEMENT_3D('',#5222,#4061,#4062);
#3550=AXIS2_PLACEMENT_3D('',#5224,#4064,#4065);
#3551=AXIS2_PLACEMENT_3D('',#5225,#4066,#4067);
#3552=AXIS2_PLACEMENT_3D('',#5263,#4069,#4070);
#3553=AXIS2_PLACEMENT_3D('',#5266,#4073,#4074);
#3554=AXIS2_PLACEMENT_3D('',#5269,#4077,#4078);
#3555=AXIS2_PLACEMENT_3D('',#5272,#4081,#4082);
#3556=AXIS2_PLACEMENT_3D('',#5275,#4085,#4086);
#3557=AXIS2_PLACEMENT_3D('',#5276,#4087,#4088);
#3558=AXIS2_PLACEMENT_3D('',#5277,#4089,#4090);
#3559=AXIS2_PLACEMENT_3D('',#5278,#4091,#4092);
#3560=AXIS2_PLACEMENT_3D('',#5279,#4093,#4094);
#3561=AXIS2_PLACEMENT_3D('',#5280,#4095,#4096);
#3562=AXIS2_PLACEMENT_3D('',#5281,#4097,#4098);
#3563=AXIS2_PLACEMENT_3D('',#5282,#4099,#4100);
#3564=AXIS2_PLACEMENT_3D('',#5291,#4105,#4106);
#3565=AXIS2_PLACEMENT_3D('',#5302,#4111,#4112);
#3566=AXIS2_PLACEMENT_3D('',#5304,#4113,#4114);
#3567=AXIS2_PLACEMENT_3D('',#5306,#4116,#4117);
#3568=AXIS2_PLACEMENT_3D('',#5317,#4122,#4123);
#3569=AXIS2_PLACEMENT_3D('',#5319,#4124,#4125);
#3570=AXIS2_PLACEMENT_3D('',#5321,#4127,#4128);
#3571=AXIS2_PLACEMENT_3D('',#5323,#4129,#4130);
#3572=AXIS2_PLACEMENT_3D('',#5327,#4132,#4133);
#3573=AXIS2_PLACEMENT_3D('',#5330,#4135,#4136);
#3574=AXIS2_PLACEMENT_3D('',#5333,#4138,#4139);
#3575=AXIS2_PLACEMENT_3D('',#5337,#4141,#4142);
#3576=AXIS2_PLACEMENT_3D('',#5340,#4144,#4145);
#3577=AXIS2_PLACEMENT_3D('',#5342,#4146,#4147);
#3578=AXIS2_PLACEMENT_3D('',#5344,#4148,#4149);
#3579=AXIS2_PLACEMENT_3D('',#5345,#4150,#4151);
#3580=AXIS2_PLACEMENT_3D('',#5350,#4153,#4154);
#3581=AXIS2_PLACEMENT_3D('',#5353,#4156,#4157);
#3582=AXIS2_PLACEMENT_3D('',#5356,#4159,#4160);
#3583=AXIS2_PLACEMENT_3D('',#5360,#4162,#4163);
#3584=AXIS2_PLACEMENT_3D('',#5363,#4165,#4166);
#3585=AXIS2_PLACEMENT_3D('',#5364,#4167,#4168);
#3586=AXIS2_PLACEMENT_3D('',#5366,#4169,#4170);
#3587=AXIS2_PLACEMENT_3D('',#5368,#4171,#4172);
#3588=AXIS2_PLACEMENT_3D('',#5369,#4173,#4174);
#3589=AXIS2_PLACEMENT_3D('',#5371,#4176,#4177);
#3590=AXIS2_PLACEMENT_3D('',#5373,#4179,#4180);
#3591=AXIS2_PLACEMENT_3D('',#5374,#4181,#4182);
#3592=AXIS2_PLACEMENT_3D('',#5412,#4184,#4185);
#3593=AXIS2_PLACEMENT_3D('',#5415,#4188,#4189);
#3594=AXIS2_PLACEMENT_3D('',#5418,#4192,#4193);
#3595=AXIS2_PLACEMENT_3D('',#5421,#4196,#4197);
#3596=AXIS2_PLACEMENT_3D('',#5424,#4200,#4201);
#3597=AXIS2_PLACEMENT_3D('',#5425,#4202,#4203);
#3598=AXIS2_PLACEMENT_3D('',#5426,#4204,#4205);
#3599=AXIS2_PLACEMENT_3D('',#5427,#4206,#4207);
#3600=AXIS2_PLACEMENT_3D('',#5428,#4208,#4209);
#3601=AXIS2_PLACEMENT_3D('',#5429,#4210,#4211);
#3602=AXIS2_PLACEMENT_3D('',#5430,#4212,#4213);
#3603=AXIS2_PLACEMENT_3D('',#5431,#4214,#4215);
#3604=AXIS2_PLACEMENT_3D('',#5440,#4220,#4221);
#3605=AXIS2_PLACEMENT_3D('',#5447,#4224,#4225);
#3606=AXIS2_PLACEMENT_3D('',#5449,#4226,#4227);
#3607=AXIS2_PLACEMENT_3D('',#5455,#4231,#4232);
#3608=AXIS2_PLACEMENT_3D('',#5462,#4235,#4236);
#3609=AXIS2_PLACEMENT_3D('',#5464,#4237,#4238);
#3610=AXIS2_PLACEMENT_3D('',#5470,#4242,#4243);
#3611=AXIS2_PLACEMENT_3D('',#5472,#4244,#4245);
#3612=AXIS2_PLACEMENT_3D('',#5476,#4247,#4248);
#3613=AXIS2_PLACEMENT_3D('',#5479,#4250,#4251);
#3614=AXIS2_PLACEMENT_3D('',#5482,#4253,#4254);
#3615=AXIS2_PLACEMENT_3D('',#5486,#4256,#4257);
#3616=AXIS2_PLACEMENT_3D('',#5489,#4259,#4260);
#3617=AXIS2_PLACEMENT_3D('',#5491,#4261,#4262);
#3618=AXIS2_PLACEMENT_3D('',#5493,#4263,#4264);
#3619=AXIS2_PLACEMENT_3D('',#5494,#4265,#4266);
#3620=AXIS2_PLACEMENT_3D('',#5498,#4268,#4269);
#3621=AXIS2_PLACEMENT_3D('',#5500,#4270,#4271);
#3622=AXIS2_PLACEMENT_3D('',#5504,#4273,#4274);
#3623=AXIS2_PLACEMENT_3D('',#5507,#4276,#4277);
#3624=AXIS2_PLACEMENT_3D('',#5510,#4279,#4280);
#3625=AXIS2_PLACEMENT_3D('',#5513,#4282,#4283);
#3626=AXIS2_PLACEMENT_3D('',#5515,#4284,#4285);
#3627=AXIS2_PLACEMENT_3D('',#5517,#4286,#4287);
#3628=AXIS2_PLACEMENT_3D('',#5518,#4288,#4289);
#3629=AXIS2_PLACEMENT_3D('',#5520,#4291,#4292);
#3630=AXIS2_PLACEMENT_3D('',#5522,#4294,#4295);
#3631=AXIS2_PLACEMENT_3D('',#5523,#4296,#4297);
#3632=AXIS2_PLACEMENT_3D('',#5561,#4299,#4300);
#3633=AXIS2_PLACEMENT_3D('',#5564,#4303,#4304);
#3634=AXIS2_PLACEMENT_3D('',#5567,#4307,#4308);
#3635=AXIS2_PLACEMENT_3D('',#5570,#4311,#4312);
#3636=AXIS2_PLACEMENT_3D('',#5573,#4315,#4316);
#3637=AXIS2_PLACEMENT_3D('',#5574,#4317,#4318);
#3638=AXIS2_PLACEMENT_3D('',#5575,#4319,#4320);
#3639=AXIS2_PLACEMENT_3D('',#5576,#4321,#4322);
#3640=AXIS2_PLACEMENT_3D('',#5577,#4323,#4324);
#3641=AXIS2_PLACEMENT_3D('',#5578,#4325,#4326);
#3642=AXIS2_PLACEMENT_3D('',#5579,#4327,#4328);
#3643=AXIS2_PLACEMENT_3D('',#5580,#4329,#4330);
#3644=AXIS2_PLACEMENT_3D('',#5589,#4335,#4336);
#3645=AXIS2_PLACEMENT_3D('',#5596,#4339,#4340);
#3646=AXIS2_PLACEMENT_3D('',#5598,#4341,#4342);
#3647=AXIS2_PLACEMENT_3D('',#5604,#4346,#4347);
#3648=AXIS2_PLACEMENT_3D('',#5611,#4350,#4351);
#3649=AXIS2_PLACEMENT_3D('',#5613,#4352,#4353);
#3650=AXIS2_PLACEMENT_3D('',#5619,#4357,#4358);
#3651=AXIS2_PLACEMENT_3D('',#5621,#4359,#4360);
#3652=AXIS2_PLACEMENT_3D('',#5625,#4362,#4363);
#3653=AXIS2_PLACEMENT_3D('',#5628,#4365,#4366);
#3654=AXIS2_PLACEMENT_3D('',#5631,#4368,#4369);
#3655=AXIS2_PLACEMENT_3D('',#5635,#4371,#4372);
#3656=AXIS2_PLACEMENT_3D('',#5638,#4374,#4375);
#3657=AXIS2_PLACEMENT_3D('',#5640,#4376,#4377);
#3658=AXIS2_PLACEMENT_3D('',#5642,#4378,#4379);
#3659=AXIS2_PLACEMENT_3D('',#5643,#4380,#4381);
#3660=AXIS2_PLACEMENT_3D('',#5647,#4383,#4384);
#3661=AXIS2_PLACEMENT_3D('',#5649,#4385,#4386);
#3662=AXIS2_PLACEMENT_3D('',#5653,#4388,#4389);
#3663=AXIS2_PLACEMENT_3D('',#5656,#4391,#4392);
#3664=AXIS2_PLACEMENT_3D('',#5659,#4394,#4395);
#3665=AXIS2_PLACEMENT_3D('',#5662,#4397,#4398);
#3666=AXIS2_PLACEMENT_3D('',#5664,#4399,#4400);
#3667=AXIS2_PLACEMENT_3D('',#5666,#4401,#4402);
#3668=AXIS2_PLACEMENT_3D('',#5667,#4403,#4404);
#3669=AXIS2_PLACEMENT_3D('',#5669,#4406,#4407);
#3670=AXIS2_PLACEMENT_3D('',#5671,#4409,#4410);
#3671=AXIS2_PLACEMENT_3D('',#5672,#4411,#4412);
#3672=AXIS2_PLACEMENT_3D('',#5710,#4414,#4415);
#3673=AXIS2_PLACEMENT_3D('',#5713,#4418,#4419);
#3674=AXIS2_PLACEMENT_3D('',#5716,#4422,#4423);
#3675=AXIS2_PLACEMENT_3D('',#5719,#4426,#4427);
#3676=AXIS2_PLACEMENT_3D('',#5722,#4430,#4431);
#3677=AXIS2_PLACEMENT_3D('',#5723,#4432,#4433);
#3678=AXIS2_PLACEMENT_3D('',#5724,#4434,#4435);
#3679=AXIS2_PLACEMENT_3D('',#5725,#4436,#4437);
#3680=AXIS2_PLACEMENT_3D('',#5726,#4438,#4439);
#3681=AXIS2_PLACEMENT_3D('',#5727,#4440,#4441);
#3682=AXIS2_PLACEMENT_3D('',#5728,#4442,#4443);
#3683=AXIS2_PLACEMENT_3D('',#5729,#4444,#4445);
#3684=AXIS2_PLACEMENT_3D('',#5730,#4446,#4447);
#3685=AXIS2_PLACEMENT_3D('',#5739,#4452,#4453);
#3686=AXIS2_PLACEMENT_3D('',#5748,#4458,#4459);
#3687=AXIS2_PLACEMENT_3D('',#5758,#4464,#4465);
#3688=AXIS2_PLACEMENT_3D('',#5760,#4466,#4467);
#3689=AXIS2_PLACEMENT_3D('',#5761,#4468,#4469);
#3690=AXIS2_PLACEMENT_3D('',#5770,#4474,#4475);
#3691=AXIS2_PLACEMENT_3D('',#5772,#4476,#4477);
#3692=AXIS2_PLACEMENT_3D('',#5775,#4479,#4480);
#3693=AXIS2_PLACEMENT_3D('',#5776,#4481,#4482);
#3694=AXIS2_PLACEMENT_3D('',#5785,#4487,#4488);
#3695=AXIS2_PLACEMENT_3D('',#5787,#4489,#4490);
#3696=AXIS2_PLACEMENT_3D('',#5790,#4492,#4493);
#3697=AXIS2_PLACEMENT_3D('',#5791,#4494,#4495);
#3698=AXIS2_PLACEMENT_3D('',#5796,#4497,#4498);
#3699=AXIS2_PLACEMENT_3D('',#5797,#4499,#4500);
#3700=AXIS2_PLACEMENT_3D('',#5798,#4501,#4502);
#3701=AXIS2_PLACEMENT_3D('',#5799,#4503,#4504);
#3702=AXIS2_PLACEMENT_3D('',#5800,#4505,#4506);
#3703=AXIS2_PLACEMENT_3D('',#5801,#4507,#4508);
#3704=AXIS2_PLACEMENT_3D('',#5803,#4509,#4510);
#3705=AXIS2_PLACEMENT_3D('',#5804,#4511,#4512);
#3706=AXIS2_PLACEMENT_3D('',#5805,#4513,#4514);
#3707=AXIS2_PLACEMENT_3D('',#5806,#4515,#4516);
#3708=AXIS2_PLACEMENT_3D('',#5807,#4517,#4518);
#3709=AXIS2_PLACEMENT_3D('',#5808,#4519,#4520);
#3710=AXIS2_PLACEMENT_3D('',#5809,#4521,#4522);
#3711=AXIS2_PLACEMENT_3D('',#5810,#4523,#4524);
#3712=AXIS2_PLACEMENT_3D('',#5811,#4525,#4526);
#3713=AXIS2_PLACEMENT_3D('',#5813,#4527,#4528);
#3714=AXIS2_PLACEMENT_3D('',#5815,#4529,#4530);
#3715=AXIS2_PLACEMENT_3D('',#5819,#4532,#4533);
#3716=AXIS2_PLACEMENT_3D('',#5820,#4534,#4535);
#3717=AXIS2_PLACEMENT_3D('',#5821,#4536,#4537);
#3718=AXIS2_PLACEMENT_3D('',#5822,#4538,#4539);
#3719=AXIS2_PLACEMENT_3D('',#5823,#4540,#4541);
#3720=AXIS2_PLACEMENT_3D('',#5824,#4542,#4543);
#3721=AXIS2_PLACEMENT_3D('',#5825,#4544,#4545);
#3722=AXIS2_PLACEMENT_3D('',#5829,#4547,#4548);
#3723=AXIS2_PLACEMENT_3D('',#5834,#4551,#4552);
#3724=AXIS2_PLACEMENT_3D('',#5836,#4553,#4554);
#3725=AXIS2_PLACEMENT_3D('',#5838,#4556,#4557);
#3726=AXIS2_PLACEMENT_3D('',#5853,#4559,#4560);
#3727=AXIS2_PLACEMENT_3D('',#5865,#4562,#4563);
#3728=AXIS2_PLACEMENT_3D('',#5867,#4565,#4566);
#3729=AXIS2_PLACEMENT_3D('',#5868,#4567,#4568);
#3730=AXIS2_PLACEMENT_3D('',#5870,#4570,#4571);
#3731=AXIS2_PLACEMENT_3D('',#5871,#4572,#4573);
#3732=AXIS2_PLACEMENT_3D('',#5872,#4574,#4575);
#3733=AXIS2_PLACEMENT_3D('',#5881,#4580,#4581);
#3734=AXIS2_PLACEMENT_3D('',#5890,#4586,#4587);
#3735=AXIS2_PLACEMENT_3D('',#5900,#4592,#4593);
#3736=AXIS2_PLACEMENT_3D('',#5902,#4594,#4595);
#3737=AXIS2_PLACEMENT_3D('',#5903,#4596,#4597);
#3738=AXIS2_PLACEMENT_3D('',#5912,#4602,#4603);
#3739=AXIS2_PLACEMENT_3D('',#5914,#4604,#4605);
#3740=AXIS2_PLACEMENT_3D('',#5917,#4607,#4608);
#3741=AXIS2_PLACEMENT_3D('',#5918,#4609,#4610);
#3742=AXIS2_PLACEMENT_3D('',#5927,#4615,#4616);
#3743=AXIS2_PLACEMENT_3D('',#5929,#4617,#4618);
#3744=AXIS2_PLACEMENT_3D('',#5932,#4620,#4621);
#3745=AXIS2_PLACEMENT_3D('',#5933,#4622,#4623);
#3746=AXIS2_PLACEMENT_3D('',#5938,#4625,#4626);
#3747=AXIS2_PLACEMENT_3D('',#5939,#4627,#4628);
#3748=AXIS2_PLACEMENT_3D('',#5940,#4629,#4630);
#3749=AXIS2_PLACEMENT_3D('',#5941,#4631,#4632);
#3750=AXIS2_PLACEMENT_3D('',#5942,#4633,#4634);
#3751=AXIS2_PLACEMENT_3D('',#5943,#4635,#4636);
#3752=AXIS2_PLACEMENT_3D('',#5945,#4637,#4638);
#3753=AXIS2_PLACEMENT_3D('',#5946,#4639,#4640);
#3754=AXIS2_PLACEMENT_3D('',#5947,#4641,#4642);
#3755=AXIS2_PLACEMENT_3D('',#5948,#4643,#4644);
#3756=AXIS2_PLACEMENT_3D('',#5949,#4645,#4646);
#3757=AXIS2_PLACEMENT_3D('',#5951,#4647,#4648);
#3758=AXIS2_PLACEMENT_3D('',#5953,#4649,#4650);
#3759=AXIS2_PLACEMENT_3D('',#5957,#4652,#4653);
#3760=AXIS2_PLACEMENT_3D('',#5958,#4654,#4655);
#3761=AXIS2_PLACEMENT_3D('',#5959,#4656,#4657);
#3762=AXIS2_PLACEMENT_3D('',#5960,#4658,#4659);
#3763=AXIS2_PLACEMENT_3D('',#5961,#4660,#4661);
#3764=AXIS2_PLACEMENT_3D('',#5962,#4662,#4663);
#3765=AXIS2_PLACEMENT_3D('',#5963,#4664,#4665);
#3766=AXIS2_PLACEMENT_3D('',#5964,#4666,#4667);
#3767=AXIS2_PLACEMENT_3D('',#5965,#4668,#4669);
#3768=AXIS2_PLACEMENT_3D('',#5966,#4670,#4671);
#3769=AXIS2_PLACEMENT_3D('',#5967,#4672,#4673);
#3770=AXIS2_PLACEMENT_3D('',#5971,#4675,#4676);
#3771=AXIS2_PLACEMENT_3D('',#5973,#4677,#4678);
#3772=AXIS2_PLACEMENT_3D('',#5978,#4681,#4682);
#3773=AXIS2_PLACEMENT_3D('',#5980,#4684,#4685);
#3774=AXIS2_PLACEMENT_3D('',#5995,#4687,#4688);
#3775=AXIS2_PLACEMENT_3D('',#6007,#4690,#4691);
#3776=AXIS2_PLACEMENT_3D('',#6009,#4693,#4694);
#3777=AXIS2_PLACEMENT_3D('',#6010,#4695,#4696);
#3778=AXIS2_PLACEMENT_3D('',#6012,#4698,#4699);
#3779=AXIS2_PLACEMENT_3D('',#6013,#4700,#4701);
#3780=AXIS2_PLACEMENT_3D('',#6014,#4702,#4703);
#3781=AXIS2_PLACEMENT_3D('',#6017,#4704,#4705);
#3782=AXIS2_PLACEMENT_3D('',#6021,#4707,#4708);
#3783=AXIS2_PLACEMENT_3D('',#6022,#4709,#4710);
#3784=AXIS2_PLACEMENT_3D('',#6023,#4711,#4712);
#3785=AXIS2_PLACEMENT_3D('',#6024,#4713,#4714);
#3786=AXIS2_PLACEMENT_3D('',#6026,#4715,#4716);
#3787=AXIS2_PLACEMENT_3D('',#6027,#4717,#4718);
#3788=AXIS2_PLACEMENT_3D('',#6029,#4719,#4720);
#3789=AXIS2_PLACEMENT_3D('',#6030,#4721,#4722);
#3790=AXIS2_PLACEMENT_3D('',#6031,#4723,#4724);
#3791=AXIS2_PLACEMENT_3D('',#6032,#4725,#4726);
#3792=AXIS2_PLACEMENT_3D('',#6033,#4727,#4728);
#3793=AXIS2_PLACEMENT_3D('',#6034,#4729,#4730);
#3794=AXIS2_PLACEMENT_3D('',#6035,#4731,#4732);
#3795=AXIS2_PLACEMENT_3D('',#6036,#4733,#4734);
#3796=AXIS2_PLACEMENT_3D('',#6037,#4735,#4736);
#3797=AXIS2_PLACEMENT_3D('',#6038,#4737,#4738);
#3798=AXIS2_PLACEMENT_3D('',#6039,#4739,#4740);
#3799=AXIS2_PLACEMENT_3D('',#6040,#4741,#4742);
#3800=AXIS2_PLACEMENT_3D('',#6041,#4743,#4744);
#3801=AXIS2_PLACEMENT_3D('',#6042,#4745,#4746);
#3802=AXIS2_PLACEMENT_3D('',#6043,#4747,#4748);
#3803=AXIS2_PLACEMENT_3D('',#6044,#4749,#4750);
#3804=AXIS2_PLACEMENT_3D('',#6045,#4751,#4752);
#3805=AXIS2_PLACEMENT_3D('',#6046,#4753,#4754);
#3806=AXIS2_PLACEMENT_3D('',#6049,#4755,#4756);
#3807=AXIS2_PLACEMENT_3D('',#6052,#4758,#4759);
#3808=AXIS2_PLACEMENT_3D('',#6053,#4760,#4761);
#3809=AXIS2_PLACEMENT_3D('',#6054,#4762,#4763);
#3810=AXIS2_PLACEMENT_3D('',#6056,#4764,#4765);
#3811=AXIS2_PLACEMENT_3D('',#6057,#4766,#4767);
#3812=AXIS2_PLACEMENT_3D('',#6060,#4769,#4770);
#3813=AXIS2_PLACEMENT_3D('',#6061,#4771,#4772);
#3814=AXIS2_PLACEMENT_3D('',#6064,#4773,#4774);
#3815=AXIS2_PLACEMENT_3D('',#6066,#4776,#4777);
#3816=AXIS2_PLACEMENT_3D('',#6067,#4778,#4779);
#3817=AXIS2_PLACEMENT_3D('',#6069,#4780,#4781);
#3818=AXIS2_PLACEMENT_3D('',#6071,#4783,#4784);
#3819=AXIS2_PLACEMENT_3D('',#6074,#4785,#4786);
#3820=AXIS2_PLACEMENT_3D('',#6077,#4788,#4789);
#3821=AXIS2_PLACEMENT_3D('',#6078,#4790,#4791);
#3822=AXIS2_PLACEMENT_3D('',#6079,#4792,#4793);
#3823=AXIS2_PLACEMENT_3D('',#6081,#4794,#4795);
#3824=AXIS2_PLACEMENT_3D('',#6082,#4796,#4797);
#3825=AXIS2_PLACEMENT_3D('',#6084,#4798,#4799);
#3826=AXIS2_PLACEMENT_3D('',#6086,#4801,#4802);
#3827=AXIS2_PLACEMENT_3D('',#6089,#4803,#4804);
#3828=AXIS2_PLACEMENT_3D('',#6091,#4806,#4807);
#3829=AXIS2_PLACEMENT_3D('',#6092,#4808,#4809);
#3830=AXIS2_PLACEMENT_3D('',#6095,#4811,#4812);
#3831=AXIS2_PLACEMENT_3D('',#6096,#4813,#4814);
#3832=AXIS2_PLACEMENT_3D('',#6098,#4815,#4816);
#3833=AXIS2_PLACEMENT_3D('',#6099,#4817,#4818);
#3834=AXIS2_PLACEMENT_3D('',#6101,#4819,#4820);
#3835=AXIS2_PLACEMENT_3D('',#6103,#4822,#4823);
#3836=AXIS2_PLACEMENT_3D('',#6105,#4824,#4825);
#3837=AXIS2_PLACEMENT_3D('',#6106,#4826,#4827);
#3838=AXIS2_PLACEMENT_3D('',#6108,#4828,#4829);
#3839=AXIS2_PLACEMENT_3D('',#6110,#4831,#4832);
#3840=AXIS2_PLACEMENT_3D('',#6112,#4833,#4834);
#3841=AXIS2_PLACEMENT_3D('',#6114,#4836,#4837);
#3842=AXIS2_PLACEMENT_3D('',#6116,#4838,#4839);
#3843=AXIS2_PLACEMENT_3D('',#6118,#4841,#4842);
#3844=AXIS2_PLACEMENT_3D('',#6121,#4844,#4845);
#3845=AXIS2_PLACEMENT_3D('',#6122,#4846,#4847);
#3846=AXIS2_PLACEMENT_3D('',#6124,#4848,#4849);
#3847=AXIS2_PLACEMENT_3D('',#6126,#4851,#4852);
#3848=AXIS2_PLACEMENT_3D('',#6128,#4853,#4854);
#3849=AXIS2_PLACEMENT_3D('',#6129,#4855,#4856);
#3850=AXIS2_PLACEMENT_3D('',#6131,#4857,#4858);
#3851=AXIS2_PLACEMENT_3D('',#6133,#4860,#4861);
#3852=AXIS2_PLACEMENT_3D('',#6134,#4862,#4863);
#3853=AXIS2_PLACEMENT_3D('',#6136,#4864,#4865);
#3854=AXIS2_PLACEMENT_3D('',#6137,#4866,#4867);
#3855=AXIS2_PLACEMENT_3D('',#6139,#4868,#4869);
#3856=AXIS2_PLACEMENT_3D('',#6141,#4871,#4872);
#3857=AXIS2_PLACEMENT_3D('',#6143,#4873,#4874);
#3858=AXIS2_PLACEMENT_3D('',#6144,#4875,#4876);
#3859=AXIS2_PLACEMENT_3D('',#6146,#4877,#4878);
#3860=AXIS2_PLACEMENT_3D('',#6148,#4880,#4881);
#3861=AXIS2_PLACEMENT_3D('',#6150,#4882,#4883);
#3862=AXIS2_PLACEMENT_3D('',#6151,#4884,#4885);
#3863=AXIS2_PLACEMENT_3D('',#6153,#4886,#4887);
#3864=AXIS2_PLACEMENT_3D('',#6155,#4889,#4890);
#3865=AXIS2_PLACEMENT_3D('',#6156,#4891,#4892);
#3866=AXIS2_PLACEMENT_3D('',#6157,#4893,#4894);
#3867=AXIS2_PLACEMENT_3D('',#6159,#4895,#4896);
#3868=AXIS2_PLACEMENT_3D('',#6161,#4897,#4898);
#3869=AXIS2_PLACEMENT_3D('',#6162,#4899,#4900);
#3870=AXIS2_PLACEMENT_3D('',#6165,#4902,#4903);
#3871=AXIS2_PLACEMENT_3D('',#6166,#4904,#4905);
#3872=AXIS2_PLACEMENT_3D('',#6168,#4906,#4907);
#3873=AXIS2_PLACEMENT_3D('',#6169,#4908,#4909);
#3874=AXIS2_PLACEMENT_3D('',#6171,#4910,#4911);
#3875=AXIS2_PLACEMENT_3D('',#6173,#4913,#4914);
#3876=AXIS2_PLACEMENT_3D('',#6176,#4916,#4917);
#3877=AXIS2_PLACEMENT_3D('',#6177,#4918,#4919);
#3878=AXIS2_PLACEMENT_3D('',#6179,#4920,#4921);
#3879=AXIS2_PLACEMENT_3D('',#6180,#4922,#4923);
#3880=AXIS2_PLACEMENT_3D('',#6182,#4925,#4926);
#3881=AXIS2_PLACEMENT_3D('',#6183,#4927,#4928);
#3882=AXIS2_PLACEMENT_3D('',#6185,#4929,#4930);
#3883=AXIS2_PLACEMENT_3D('',#6187,#4931,#4932);
#3884=AXIS2_PLACEMENT_3D('',#6188,#4933,#4934);
#3885=AXIS2_PLACEMENT_3D('',#6190,#4935,#4936);
#3886=AXIS2_PLACEMENT_3D('',#6192,#4938,#4939);
#3887=AXIS2_PLACEMENT_3D('',#6194,#4940,#4941);
#3888=AXIS2_PLACEMENT_3D('',#6195,#4942,#4943);
#3889=AXIS2_PLACEMENT_3D('',#6197,#4944,#4945);
#3890=AXIS2_PLACEMENT_3D('',#6199,#4947,#4948);
#3891=AXIS2_PLACEMENT_3D('',#6201,#4949,#4950);
#3892=AXIS2_PLACEMENT_3D('',#6203,#4952,#4953);
#3893=AXIS2_PLACEMENT_3D('',#6205,#4954,#4955);
#3894=AXIS2_PLACEMENT_3D('',#6206,#4956,#4957);
#3895=AXIS2_PLACEMENT_3D('',#6208,#4959,#4960);
#3896=AXIS2_PLACEMENT_3D('',#6209,#4961,#4962);
#3897=AXIS2_PLACEMENT_3D('',#6211,#4963,#4964);
#3898=AXIS2_PLACEMENT_3D('',#6213,#4965,#4966);
#3899=AXIS2_PLACEMENT_3D('',#6214,#4967,#4968);
#3900=AXIS2_PLACEMENT_3D('',#6217,#4970,#4971);
#3901=AXIS2_PLACEMENT_3D('',#6218,#4972,#4973);
#3902=AXIS2_PLACEMENT_3D('',#6220,#4974,#4975);
#3903=AXIS2_PLACEMENT_3D('',#6221,#4976,#4977);
#3904=AXIS2_PLACEMENT_3D('',#6223,#4979,#4980);
#3905=AXIS2_PLACEMENT_3D('',#6224,#4981,#4982);
#3906=AXIS2_PLACEMENT_3D('',#6225,#4983,#4984);
#3907=AXIS2_PLACEMENT_3D('',#6226,#4985,#4986);
#3908=AXIS2_PLACEMENT_3D('',#6227,#4987,#4988);
#3909=AXIS2_PLACEMENT_3D('',#6228,#4989,#4990);
#3910=AXIS2_PLACEMENT_3D('',#6229,#4991,#4992);
#3911=AXIS2_PLACEMENT_3D('',#6230,#4993,#4994);
#3912=AXIS2_PLACEMENT_3D('',#6231,#4995,#4996);
#3913=AXIS2_PLACEMENT_3D('',#6232,#4997,#4998);
#3914=AXIS2_PLACEMENT_3D('',#6233,#4999,#5000);
#3915=AXIS2_PLACEMENT_3D('',#6234,#5001,#5002);
#3916=AXIS2_PLACEMENT_3D('',#6235,#5003,#5004);
#3917=AXIS2_PLACEMENT_3D('',#6236,#5005,#5006);
#3918=AXIS2_PLACEMENT_3D('',#6237,#5007,#5008);
#3919=AXIS2_PLACEMENT_3D('',#6238,#5009,#5010);
#3920=AXIS2_PLACEMENT_3D('',#6239,#5011,#5012);
#3921=AXIS2_PLACEMENT_3D('',#6240,#5013,#5014);
#3922=AXIS2_PLACEMENT_3D('',#6241,#5015,#5016);
#3923=AXIS2_PLACEMENT_3D('',#6242,#5017,#5018);
#3924=AXIS2_PLACEMENT_3D('',#6243,#5019,#5020);
#3925=AXIS2_PLACEMENT_3D('',#6244,#5021,#5022);
#3926=AXIS2_PLACEMENT_3D('',#6245,#5023,#5024);
#3927=AXIS2_PLACEMENT_3D('',#6246,#5025,#5026);
#3928=AXIS2_PLACEMENT_3D('',#6247,#5027,#5028);
#3929=AXIS2_PLACEMENT_3D('',#6248,#5029,#5030);
#3930=AXIS2_PLACEMENT_3D('',#6249,#5031,#5032);
#3931=AXIS2_PLACEMENT_3D('',#6250,#5033,#5034);
#3932=AXIS2_PLACEMENT_3D('',#6251,#5035,#5036);
#3933=AXIS2_PLACEMENT_3D('',#6252,#5037,#5038);
#3934=AXIS2_PLACEMENT_3D('',#6253,#5039,#5040);
#3935=AXIS2_PLACEMENT_3D('',#6254,#5041,#5042);
#3936=AXIS2_PLACEMENT_3D('',#6255,#5043,#5044);
#3937=AXIS2_PLACEMENT_3D('',#6256,#5045,#5046);
#3938=AXIS2_PLACEMENT_3D('',#6257,#5047,#5048);
#3939=AXIS2_PLACEMENT_3D('',#6258,#5049,#5050);
#3940=AXIS2_PLACEMENT_3D('',#6259,#5051,#5052);
#3941=AXIS2_PLACEMENT_3D('',#6260,#5053,#5054);
#3942=AXIS2_PLACEMENT_3D('',#6261,#5055,#5056);
#3943=AXIS2_PLACEMENT_3D('',#6262,#5057,#5058);
#3944=AXIS2_PLACEMENT_3D('',#6263,#5059,#5060);
#3945=AXIS2_PLACEMENT_3D('',#6264,#5061,#5062);
#3946=AXIS2_PLACEMENT_3D('',#6265,#5063,#5064);
#3947=AXIS2_PLACEMENT_3D('',#6266,#5065,#5066);
#3948=AXIS2_PLACEMENT_3D('',#6267,#5067,#5068);
#3949=AXIS2_PLACEMENT_3D('',#6268,#5069,#5070);
#3950=AXIS2_PLACEMENT_3D('',#6269,#5071,#5072);
#3951=AXIS2_PLACEMENT_3D('',#6270,#5073,#5074);
#3952=AXIS2_PLACEMENT_3D('',#6271,#5075,#5076);
#3953=AXIS2_PLACEMENT_3D('',#6272,#5077,#5078);
#3954=AXIS2_PLACEMENT_3D('',#6273,#5079,#5080);
#3955=AXIS2_PLACEMENT_3D('',#6274,#5081,#5082);
#3956=AXIS2_PLACEMENT_3D('',#6275,#5083,#5084);
#3957=AXIS2_PLACEMENT_3D('',#6276,#5085,#5086);
#3958=AXIS2_PLACEMENT_3D('',#6277,#5087,#5088);
#3959=AXIS2_PLACEMENT_3D('',#6278,#5089,#5090);
#3960=AXIS2_PLACEMENT_3D('',#6279,#5091,#5092);
#3961=AXIS2_PLACEMENT_3D('',#6280,#5093,#5094);
#3962=AXIS2_PLACEMENT_3D('',#6281,#5095,#5096);
#3963=AXIS2_PLACEMENT_3D('',#6282,#5097,#5098);
#3964=AXIS2_PLACEMENT_3D('',#6283,#5099,#5100);
#3965=AXIS2_PLACEMENT_3D('',#6284,#5101,#5102);
#3966=AXIS2_PLACEMENT_3D('',#6285,#5103,#5104);
#3967=AXIS2_PLACEMENT_3D('',#6286,#5105,#5106);
#3968=AXIS2_PLACEMENT_3D('',#6287,#5107,#5108);
#3969=AXIS2_PLACEMENT_3D('',#6288,#5109,#5110);
#3970=AXIS2_PLACEMENT_3D('',#6289,#5111,#5112);
#3971=AXIS2_PLACEMENT_3D('',#6290,#5113,#5114);
#3972=AXIS2_PLACEMENT_3D('',#6291,#5115,#5116);
#3973=AXIS2_PLACEMENT_3D('',#6292,#5117,#5118);
#3974=AXIS2_PLACEMENT_3D('',#6293,#5119,#5120);
#3975=AXIS2_PLACEMENT_3D('',#6294,#5121,#5122);
#3976=AXIS2_PLACEMENT_3D('',#6295,#5123,#5124);
#3977=AXIS2_PLACEMENT_3D('',#6296,#5125,#5126);
#3978=AXIS2_PLACEMENT_3D('',#6297,#5127,#5128);
#3979=AXIS2_PLACEMENT_3D('',#6298,#5129,#5130);
#3980=DIRECTION('axis',(0.,0.,1.));
#3981=DIRECTION('refdir',(1.,0.,0.));
#3982=DIRECTION('axis',(0.,0.,1.));
#3983=DIRECTION('refdir',(1.,0.,0.));
#3984=DIRECTION('center_axis',(-1.,0.,0.));
#3985=DIRECTION('ref_axis',(0.,0.,-1.));
#3986=DIRECTION('',(0.,-8.57182693503055E-17,-1.));
#3987=DIRECTION('',(0.,-1.,8.57182693503055E-17));
#3988=DIRECTION('',(0.,-8.57182693503055E-17,-1.));
#3989=DIRECTION('',(0.,-1.,8.57182693503055E-17));
#3990=DIRECTION('center_axis',(0.,8.57182693503055E-17,1.));
#3991=DIRECTION('ref_axis',(0.,-1.,8.57182693503055E-17));
#3992=DIRECTION('',(-1.,0.,0.));
#3993=DIRECTION('',(0.,1.,-8.57182693503055E-17));
#3994=DIRECTION('',(-1.,0.,0.));
#3995=DIRECTION('',(0.,-1.,8.57182693503055E-17));
#3996=DIRECTION('center_axis',(0.,-8.57182693503055E-17,-1.));
#3997=DIRECTION('ref_axis',(0.,-1.,8.57182693503055E-17));
#3998=DIRECTION('center_axis',(0.,-8.57182693503055E-17,-1.));
#3999=DIRECTION('ref_axis',(0.,-1.,8.57182693503055E-17));
#4000=DIRECTION('',(0.,-1.,8.57182693503055E-17));
#4001=DIRECTION('center_axis',(0.,8.57182693503055E-17,1.));
#4002=DIRECTION('ref_axis',(0.,-1.,8.57182693503055E-17));
#4003=DIRECTION('',(-1.,0.,0.));
#4004=DIRECTION('',(0.,1.,-8.57182693503055E-17));
#4005=DIRECTION('',(-1.,0.,0.));
#4006=DIRECTION('',(0.,-1.,8.57182693503055E-17));
#4007=DIRECTION('center_axis',(0.,-8.57182693503055E-17,-1.));
#4008=DIRECTION('ref_axis',(0.,-1.,8.57182693503055E-17));
#4009=DIRECTION('center_axis',(0.,-8.57182693503055E-17,-1.));
#4010=DIRECTION('ref_axis',(0.,-1.,8.57182693503055E-17));
#4011=DIRECTION('',(0.,-1.,8.57182693503055E-17));
#4012=DIRECTION('center_axis',(0.,-1.,8.57182693503055E-17));
#4013=DIRECTION('ref_axis',(-1.,0.,0.));
#4014=DIRECTION('center_axis',(0.,1.,-8.57182693503055E-17));
#4015=DIRECTION('ref_axis',(0.,-8.57182693503055E-17,-1.));
#4016=DIRECTION('',(-1.,0.,0.));
#4017=DIRECTION('center_axis',(0.,1.,-8.57182693503055E-17));
#4018=DIRECTION('ref_axis',(0.,-8.57182693503055E-17,-1.));
#4019=DIRECTION('',(0.,-8.57182693503055E-17,-1.));
#4020=DIRECTION('center_axis',(0.,1.,-8.57182693503055E-17));
#4021=DIRECTION('ref_axis',(0.,-8.57182693503055E-17,-1.));
#4022=DIRECTION('',(0.,-8.57182693503055E-17,-1.));
#4023=DIRECTION('center_axis',(0.,1.,-8.57182693503055E-17));
#4024=DIRECTION('ref_axis',(0.,-8.57182693503055E-17,-1.));
#4025=DIRECTION('',(0.,8.57182693503055E-17,1.));
#4026=DIRECTION('center_axis',(0.,1.,-8.57182693503055E-17));
#4027=DIRECTION('ref_axis',(0.,-8.57182693503055E-17,-1.));
#4028=DIRECTION('',(-1.,0.,0.));
#4029=DIRECTION('center_axis',(0.,1.,-8.57182693503055E-17));
#4030=DIRECTION('ref_axis',(0.,-8.57182693503055E-17,-1.));
#4031=DIRECTION('center_axis',(0.,1.,-8.57182693503055E-17));
#4032=DIRECTION('ref_axis',(0.,-8.57182693503055E-17,-1.));
#4033=DIRECTION('center_axis',(0.,1.,-8.57182693503055E-17));
#4034=DIRECTION('ref_axis',(0.,-8.57182693503055E-17,-1.));
#4035=DIRECTION('center_axis',(0.,-1.,8.57182693503055E-17));
#4036=DIRECTION('ref_axis',(-1.,0.,0.));
#4037=DIRECTION('',(-1.,0.,0.));
#4038=DIRECTION('center_axis',(0.,1.,-8.57182693503055E-17));
#4039=DIRECTION('ref_axis',(0.,-8.57182693503055E-17,-1.));
#4040=DIRECTION('',(0.,8.57182693503055E-17,1.));
#4041=DIRECTION('center_axis',(0.,1.,-8.57182693503055E-17));
#4042=DIRECTION('ref_axis',(0.,-8.57182693503055E-17,-1.));
#4043=DIRECTION('',(0.,-8.57182693503055E-17,-1.));
#4044=DIRECTION('center_axis',(0.,1.,-8.57182693503055E-17));
#4045=DIRECTION('ref_axis',(0.,-8.57182693503055E-17,-1.));
#4046=DIRECTION('',(0.,-8.57182693503055E-17,-1.));
#4047=DIRECTION('center_axis',(0.,1.,-8.57182693503055E-17));
#4048=DIRECTION('ref_axis',(0.,-8.57182693503055E-17,-1.));
#4049=DIRECTION('',(-1.,0.,0.));
#4050=DIRECTION('center_axis',(0.,1.,-8.57182693503055E-17));
#4051=DIRECTION('ref_axis',(0.,-8.57182693503055E-17,-1.));
#4052=DIRECTION('center_axis',(0.,1.,-8.57182693503055E-17));
#4053=DIRECTION('ref_axis',(0.,-8.57182693503055E-17,-1.));
#4054=DIRECTION('center_axis',(0.,1.,-8.57182693503055E-17));
#4055=DIRECTION('ref_axis',(0.,-8.57182693503055E-17,-1.));
#4056=DIRECTION('center_axis',(0.,1.,-8.57182693503055E-17));
#4057=DIRECTION('ref_axis',(0.,-8.57182693503055E-17,-1.));
#4058=DIRECTION('center_axis',(0.,1.,-8.57182693503055E-17));
#4059=DIRECTION('ref_axis',(0.,8.57182693503055E-17,1.));
#4060=DIRECTION('',(0.,1.,-8.57182693503055E-17));
#4061=DIRECTION('center_axis',(0.,1.,-8.57182693503055E-17));
#4062=DIRECTION('ref_axis',(0.,8.57182693503055E-17,1.));
#4063=DIRECTION('',(0.,1.,-8.57182693503055E-17));
#4064=DIRECTION('center_axis',(-1.,0.,0.));
#4065=DIRECTION('ref_axis',(0.,0.,-1.));
#4066=DIRECTION('center_axis',(0.,8.57182693503055E-17,1.));
#4067=DIRECTION('ref_axis',(0.,-1.,8.57182693503055E-17));
#4068=DIRECTION('',(0.,8.57182693503055E-17,1.));
#4069=DIRECTION('center_axis',(0.,-8.57182693503055E-17,-1.));
#4070=DIRECTION('ref_axis',(0.,1.,-8.57182693503055E-17));
#4071=DIRECTION('',(0.,-1.,8.57182693503055E-17));
#4072=DIRECTION('',(0.,-1.,8.57182693503055E-17));
#4073=DIRECTION('center_axis',(-1.,0.,0.));
#4074=DIRECTION('ref_axis',(0.,0.,-1.));
#4075=DIRECTION('',(0.,-1.,8.57182693503055E-17));
#4076=DIRECTION('',(0.,-1.,8.57182693503055E-17));
#4077=DIRECTION('center_axis',(0.,-8.57182693503055E-17,-1.));
#4078=DIRECTION('ref_axis',(0.,1.,-8.57182693503055E-17));
#4079=DIRECTION('',(0.,-1.,8.57182693503055E-17));
#4080=DIRECTION('',(0.,-1.,8.57182693503055E-17));
#4081=DIRECTION('center_axis',(1.,0.,0.));
#4082=DIRECTION('ref_axis',(0.,0.,1.));
#4083=DIRECTION('',(0.,-1.,8.57182693503055E-17));
#4084=DIRECTION('',(0.,-1.,8.57182693503055E-17));
#4085=DIRECTION('center_axis',(0.,1.,-8.57182693503055E-17));
#4086=DIRECTION('ref_axis',(0.,8.57182693503055E-17,1.));
#4087=DIRECTION('center_axis',(0.,-1.,8.57182693503055E-17));
#4088=DIRECTION('ref_axis',(0.,-8.57182693503055E-17,-1.));
#4089=DIRECTION('center_axis',(0.,-1.,8.57182693503055E-17));
#4090=DIRECTION('ref_axis',(0.,-8.57182693503055E-17,-1.));
#4091=DIRECTION('center_axis',(0.,-1.,8.57182693503055E-17));
#4092=DIRECTION('ref_axis',(0.,-8.57182693503055E-17,-1.));
#4093=DIRECTION('center_axis',(0.,-1.,8.57182693503055E-17));
#4094=DIRECTION('ref_axis',(0.,-8.57182693503055E-17,-1.));
#4095=DIRECTION('center_axis',(0.,-1.,8.57182693503055E-17));
#4096=DIRECTION('ref_axis',(0.,-8.57182693503055E-17,-1.));
#4097=DIRECTION('axis',(0.,0.,1.));
#4098=DIRECTION('refdir',(1.,0.,0.));
#4099=DIRECTION('center_axis',(1.,0.,0.));
#4100=DIRECTION('ref_axis',(0.,0.,-1.));
#4101=DIRECTION('',(0.,8.57182693503055E-17,-1.));
#4102=DIRECTION('',(0.,1.,8.57182693503055E-17));
#4103=DIRECTION('',(0.,8.57182693503055E-17,-1.));
#4104=DIRECTION('',(0.,1.,8.57182693503055E-17));
#4105=DIRECTION('center_axis',(0.,-8.57182693503055E-17,1.));
#4106=DIRECTION('ref_axis',(0.,1.,8.57182693503055E-17));
#4107=DIRECTION('',(1.,0.,0.));
#4108=DIRECTION('',(0.,-1.,-8.57182693503055E-17));
#4109=DIRECTION('',(1.,0.,0.));
#4110=DIRECTION('',(0.,1.,8.57182693503055E-17));
#4111=DIRECTION('center_axis',(0.,8.57182693503055E-17,-1.));
#4112=DIRECTION('ref_axis',(0.,1.,8.57182693503055E-17));
#4113=DIRECTION('center_axis',(0.,8.57182693503055E-17,-1.));
#4114=DIRECTION('ref_axis',(0.,1.,8.57182693503055E-17));
#4115=DIRECTION('',(0.,1.,8.57182693503055E-17));
#4116=DIRECTION('center_axis',(0.,-8.57182693503055E-17,1.));
#4117=DIRECTION('ref_axis',(0.,1.,8.57182693503055E-17));
#4118=DIRECTION('',(1.,0.,0.));
#4119=DIRECTION('',(0.,-1.,-8.57182693503055E-17));
#4120=DIRECTION('',(1.,0.,0.));
#4121=DIRECTION('',(0.,1.,8.57182693503055E-17));
#4122=DIRECTION('center_axis',(0.,8.57182693503055E-17,-1.));
#4123=DIRECTION('ref_axis',(0.,1.,8.57182693503055E-17));
#4124=DIRECTION('center_axis',(0.,8.57182693503055E-17,-1.));
#4125=DIRECTION('ref_axis',(0.,1.,8.57182693503055E-17));
#4126=DIRECTION('',(0.,1.,8.57182693503055E-17));
#4127=DIRECTION('center_axis',(0.,1.,8.57182693503055E-17));
#4128=DIRECTION('ref_axis',(1.,0.,0.));
#4129=DIRECTION('center_axis',(0.,-1.,-8.57182693503055E-17));
#4130=DIRECTION('ref_axis',(0.,8.57182693503055E-17,-1.));
#4131=DIRECTION('',(1.,0.,0.));
#4132=DIRECTION('center_axis',(0.,-1.,-8.57182693503055E-17));
#4133=DIRECTION('ref_axis',(0.,8.57182693503055E-17,-1.));
#4134=DIRECTION('',(0.,8.57182693503055E-17,-1.));
#4135=DIRECTION('center_axis',(0.,-1.,-8.57182693503055E-17));
#4136=DIRECTION('ref_axis',(0.,8.57182693503055E-17,-1.));
#4137=DIRECTION('',(0.,8.57182693503055E-17,-1.));
#4138=DIRECTION('center_axis',(0.,-1.,-8.57182693503055E-17));
#4139=DIRECTION('ref_axis',(0.,8.57182693503055E-17,-1.));
#4140=DIRECTION('',(0.,-8.57182693503055E-17,1.));
#4141=DIRECTION('center_axis',(0.,-1.,-8.57182693503055E-17));
#4142=DIRECTION('ref_axis',(0.,8.57182693503055E-17,-1.));
#4143=DIRECTION('',(1.,0.,0.));
#4144=DIRECTION('center_axis',(0.,-1.,-8.57182693503055E-17));
#4145=DIRECTION('ref_axis',(0.,8.57182693503055E-17,-1.));
#4146=DIRECTION('center_axis',(0.,-1.,-8.57182693503055E-17));
#4147=DIRECTION('ref_axis',(0.,8.57182693503055E-17,-1.));
#4148=DIRECTION('center_axis',(0.,-1.,-8.57182693503055E-17));
#4149=DIRECTION('ref_axis',(0.,8.57182693503055E-17,-1.));
#4150=DIRECTION('center_axis',(0.,1.,8.57182693503055E-17));
#4151=DIRECTION('ref_axis',(1.,0.,0.));
#4152=DIRECTION('',(1.,0.,0.));
#4153=DIRECTION('center_axis',(0.,-1.,-8.57182693503055E-17));
#4154=DIRECTION('ref_axis',(0.,8.57182693503055E-17,-1.));
#4155=DIRECTION('',(0.,-8.57182693503055E-17,1.));
#4156=DIRECTION('center_axis',(0.,-1.,-8.57182693503055E-17));
#4157=DIRECTION('ref_axis',(0.,8.57182693503055E-17,-1.));
#4158=DIRECTION('',(0.,8.57182693503055E-17,-1.));
#4159=DIRECTION('center_axis',(0.,-1.,-8.57182693503055E-17));
#4160=DIRECTION('ref_axis',(0.,8.57182693503055E-17,-1.));
#4161=DIRECTION('',(0.,8.57182693503055E-17,-1.));
#4162=DIRECTION('center_axis',(0.,-1.,-8.57182693503055E-17));
#4163=DIRECTION('ref_axis',(0.,8.57182693503055E-17,-1.));
#4164=DIRECTION('',(1.,0.,0.));
#4165=DIRECTION('center_axis',(0.,-1.,-8.57182693503055E-17));
#4166=DIRECTION('ref_axis',(0.,8.57182693503055E-17,-1.));
#4167=DIRECTION('center_axis',(0.,-1.,-8.57182693503055E-17));
#4168=DIRECTION('ref_axis',(0.,8.57182693503055E-17,-1.));
#4169=DIRECTION('center_axis',(0.,-1.,-8.57182693503055E-17));
#4170=DIRECTION('ref_axis',(0.,8.57182693503055E-17,-1.));
#4171=DIRECTION('center_axis',(0.,-1.,-8.57182693503055E-17));
#4172=DIRECTION('ref_axis',(0.,8.57182693503055E-17,-1.));
#4173=DIRECTION('center_axis',(0.,-1.,-8.57182693503055E-17));
#4174=DIRECTION('ref_axis',(0.,-8.57182693503055E-17,1.));
#4175=DIRECTION('',(0.,-1.,-8.57182693503055E-17));
#4176=DIRECTION('center_axis',(0.,-1.,-8.57182693503055E-17));
#4177=DIRECTION('ref_axis',(0.,-8.57182693503055E-17,1.));
#4178=DIRECTION('',(0.,-1.,-8.57182693503055E-17));
#4179=DIRECTION('center_axis',(1.,0.,0.));
#4180=DIRECTION('ref_axis',(0.,0.,-1.));
#4181=DIRECTION('center_axis',(0.,-8.57182693503055E-17,1.));
#4182=DIRECTION('ref_axis',(0.,1.,8.57182693503055E-17));
#4183=DIRECTION('',(0.,-8.57182693503055E-17,1.));
#4184=DIRECTION('center_axis',(0.,8.57182693503055E-17,-1.));
#4185=DIRECTION('ref_axis',(0.,-1.,-8.57182693503055E-17));
#4186=DIRECTION('',(0.,1.,8.57182693503055E-17));
#4187=DIRECTION('',(0.,1.,8.57182693503055E-17));
#4188=DIRECTION('center_axis',(1.,0.,0.));
#4189=DIRECTION('ref_axis',(0.,0.,-1.));
#4190=DIRECTION('',(0.,1.,8.57182693503055E-17));
#4191=DIRECTION('',(0.,1.,8.57182693503055E-17));
#4192=DIRECTION('center_axis',(0.,8.57182693503055E-17,-1.));
#4193=DIRECTION('ref_axis',(0.,-1.,-8.57182693503055E-17));
#4194=DIRECTION('',(0.,1.,8.57182693503055E-17));
#4195=DIRECTION('',(0.,1.,8.57182693503055E-17));
#4196=DIRECTION('center_axis',(-1.,0.,0.));
#4197=DIRECTION('ref_axis',(0.,0.,1.));
#4198=DIRECTION('',(0.,1.,8.57182693503055E-17));
#4199=DIRECTION('',(0.,1.,8.57182693503055E-17));
#4200=DIRECTION('center_axis',(0.,-1.,-8.57182693503055E-17));
#4201=DIRECTION('ref_axis',(0.,-8.57182693503055E-17,1.));
#4202=DIRECTION('center_axis',(0.,1.,8.57182693503055E-17));
#4203=DIRECTION('ref_axis',(0.,8.57182693503055E-17,-1.));
#4204=DIRECTION('center_axis',(0.,1.,8.57182693503055E-17));
#4205=DIRECTION('ref_axis',(0.,8.57182693503055E-17,-1.));
#4206=DIRECTION('center_axis',(0.,1.,8.57182693503055E-17));
#4207=DIRECTION('ref_axis',(0.,8.57182693503055E-17,-1.));
#4208=DIRECTION('center_axis',(0.,1.,8.57182693503055E-17));
#4209=DIRECTION('ref_axis',(0.,8.57182693503055E-17,-1.));
#4210=DIRECTION('center_axis',(0.,1.,8.57182693503055E-17));
#4211=DIRECTION('ref_axis',(0.,8.57182693503055E-17,-1.));
#4212=DIRECTION('axis',(0.,0.,1.));
#4213=DIRECTION('refdir',(1.,0.,0.));
#4214=DIRECTION('center_axis',(1.,0.,0.));
#4215=DIRECTION('ref_axis',(0.,0.,-1.));
#4216=DIRECTION('',(0.,-8.57182693503055E-17,-1.));
#4217=DIRECTION('',(0.,-1.,8.57182693503055E-17));
#4218=DIRECTION('',(0.,-8.57182693503055E-17,-1.));
#4219=DIRECTION('',(0.,-1.,8.57182693503055E-17));
#4220=DIRECTION('center_axis',(0.,8.57182693503055E-17,1.));
#4221=DIRECTION('ref_axis',(0.,-1.,8.57182693503055E-17));
#4222=DIRECTION('',(1.,0.,0.));
#4223=DIRECTION('',(0.,-1.,8.57182693503055E-17));
#4224=DIRECTION('center_axis',(0.,8.57182693503055E-17,1.));
#4225=DIRECTION('ref_axis',(0.,-1.,8.57182693503055E-17));
#4226=DIRECTION('center_axis',(0.,8.57182693503055E-17,1.));
#4227=DIRECTION('ref_axis',(0.,-1.,8.57182693503055E-17));
#4228=DIRECTION('',(0.,-1.,8.57182693503055E-17));
#4229=DIRECTION('',(1.,0.,0.));
#4230=DIRECTION('',(0.,1.,-8.57182693503055E-17));
#4231=DIRECTION('center_axis',(0.,8.57182693503055E-17,1.));
#4232=DIRECTION('ref_axis',(0.,-1.,8.57182693503055E-17));
#4233=DIRECTION('',(1.,0.,0.));
#4234=DIRECTION('',(0.,-1.,8.57182693503055E-17));
#4235=DIRECTION('center_axis',(0.,8.57182693503055E-17,1.));
#4236=DIRECTION('ref_axis',(0.,-1.,8.57182693503055E-17));
#4237=DIRECTION('center_axis',(0.,8.57182693503055E-17,1.));
#4238=DIRECTION('ref_axis',(0.,-1.,8.57182693503055E-17));
#4239=DIRECTION('',(0.,-1.,8.57182693503055E-17));
#4240=DIRECTION('',(1.,0.,0.));
#4241=DIRECTION('',(0.,1.,-8.57182693503055E-17));
#4242=DIRECTION('center_axis',(0.,-1.,8.57182693503055E-17));
#4243=DIRECTION('ref_axis',(1.,0.,0.));
#4244=DIRECTION('center_axis',(0.,-1.,8.57182693503055E-17));
#4245=DIRECTION('ref_axis',(0.,-8.57182693503055E-17,-1.));
#4246=DIRECTION('',(1.,0.,0.));
#4247=DIRECTION('center_axis',(0.,-1.,8.57182693503055E-17));
#4248=DIRECTION('ref_axis',(0.,-8.57182693503055E-17,-1.));
#4249=DIRECTION('',(0.,8.57182693503055E-17,1.));
#4250=DIRECTION('center_axis',(0.,-1.,8.57182693503055E-17));
#4251=DIRECTION('ref_axis',(0.,-8.57182693503055E-17,-1.));
#4252=DIRECTION('',(0.,-8.57182693503055E-17,-1.));
#4253=DIRECTION('center_axis',(0.,-1.,8.57182693503055E-17));
#4254=DIRECTION('ref_axis',(0.,-8.57182693503055E-17,-1.));
#4255=DIRECTION('',(0.,-8.57182693503055E-17,-1.));
#4256=DIRECTION('center_axis',(0.,-1.,8.57182693503055E-17));
#4257=DIRECTION('ref_axis',(0.,-8.57182693503055E-17,-1.));
#4258=DIRECTION('',(1.,0.,0.));
#4259=DIRECTION('center_axis',(0.,-1.,8.57182693503055E-17));
#4260=DIRECTION('ref_axis',(0.,-8.57182693503055E-17,-1.));
#4261=DIRECTION('center_axis',(0.,-1.,8.57182693503055E-17));
#4262=DIRECTION('ref_axis',(0.,-8.57182693503055E-17,-1.));
#4263=DIRECTION('center_axis',(0.,-1.,8.57182693503055E-17));
#4264=DIRECTION('ref_axis',(0.,-8.57182693503055E-17,-1.));
#4265=DIRECTION('center_axis',(0.,-1.,8.57182693503055E-17));
#4266=DIRECTION('ref_axis',(1.,0.,0.));
#4267=DIRECTION('',(1.,0.,0.));
#4268=DIRECTION('center_axis',(0.,-1.,8.57182693503055E-17));
#4269=DIRECTION('ref_axis',(0.,-8.57182693503055E-17,-1.));
#4270=DIRECTION('center_axis',(0.,-1.,8.57182693503055E-17));
#4271=DIRECTION('ref_axis',(0.,-8.57182693503055E-17,-1.));
#4272=DIRECTION('',(1.,0.,0.));
#4273=DIRECTION('center_axis',(0.,-1.,8.57182693503055E-17));
#4274=DIRECTION('ref_axis',(0.,-8.57182693503055E-17,-1.));
#4275=DIRECTION('',(0.,-8.57182693503055E-17,-1.));
#4276=DIRECTION('center_axis',(0.,-1.,8.57182693503055E-17));
#4277=DIRECTION('ref_axis',(0.,-8.57182693503055E-17,-1.));
#4278=DIRECTION('',(0.,-8.57182693503055E-17,-1.));
#4279=DIRECTION('center_axis',(0.,-1.,8.57182693503055E-17));
#4280=DIRECTION('ref_axis',(0.,-8.57182693503055E-17,-1.));
#4281=DIRECTION('',(0.,8.57182693503055E-17,1.));
#4282=DIRECTION('center_axis',(0.,-1.,8.57182693503055E-17));
#4283=DIRECTION('ref_axis',(0.,-8.57182693503055E-17,-1.));
#4284=DIRECTION('center_axis',(0.,-1.,8.57182693503055E-17));
#4285=DIRECTION('ref_axis',(0.,-8.57182693503055E-17,-1.));
#4286=DIRECTION('center_axis',(0.,-1.,8.57182693503055E-17));
#4287=DIRECTION('ref_axis',(0.,-8.57182693503055E-17,-1.));
#4288=DIRECTION('center_axis',(0.,1.,-8.57182693503055E-17));
#4289=DIRECTION('ref_axis',(0.,8.57182693503055E-17,1.));
#4290=DIRECTION('',(0.,1.,-8.57182693503055E-17));
#4291=DIRECTION('center_axis',(0.,1.,-8.57182693503055E-17));
#4292=DIRECTION('ref_axis',(0.,8.57182693503055E-17,1.));
#4293=DIRECTION('',(0.,1.,-8.57182693503055E-17));
#4294=DIRECTION('center_axis',(1.,0.,0.));
#4295=DIRECTION('ref_axis',(0.,0.,-1.));
#4296=DIRECTION('center_axis',(0.,8.57182693503055E-17,1.));
#4297=DIRECTION('ref_axis',(0.,-1.,8.57182693503055E-17));
#4298=DIRECTION('',(0.,8.57182693503055E-17,1.));
#4299=DIRECTION('center_axis',(0.,-8.57182693503055E-17,-1.));
#4300=DIRECTION('ref_axis',(0.,1.,-8.57182693503055E-17));
#4301=DIRECTION('',(0.,-1.,8.57182693503055E-17));
#4302=DIRECTION('',(0.,-1.,8.57182693503055E-17));
#4303=DIRECTION('center_axis',(1.,0.,0.));
#4304=DIRECTION('ref_axis',(0.,0.,-1.));
#4305=DIRECTION('',(0.,-1.,8.57182693503055E-17));
#4306=DIRECTION('',(0.,-1.,8.57182693503055E-17));
#4307=DIRECTION('center_axis',(0.,-8.57182693503055E-17,-1.));
#4308=DIRECTION('ref_axis',(0.,1.,-8.57182693503055E-17));
#4309=DIRECTION('',(0.,-1.,8.57182693503055E-17));
#4310=DIRECTION('',(0.,-1.,8.57182693503055E-17));
#4311=DIRECTION('center_axis',(-1.,0.,0.));
#4312=DIRECTION('ref_axis',(0.,0.,1.));
#4313=DIRECTION('',(0.,-1.,8.57182693503055E-17));
#4314=DIRECTION('',(0.,-1.,8.57182693503055E-17));
#4315=DIRECTION('center_axis',(0.,1.,-8.57182693503055E-17));
#4316=DIRECTION('ref_axis',(0.,8.57182693503055E-17,1.));
#4317=DIRECTION('center_axis',(0.,-1.,8.57182693503055E-17));
#4318=DIRECTION('ref_axis',(0.,-8.57182693503055E-17,-1.));
#4319=DIRECTION('center_axis',(0.,-1.,8.57182693503055E-17));
#4320=DIRECTION('ref_axis',(0.,-8.57182693503055E-17,-1.));
#4321=DIRECTION('center_axis',(0.,-1.,8.57182693503055E-17));
#4322=DIRECTION('ref_axis',(0.,-8.57182693503055E-17,-1.));
#4323=DIRECTION('center_axis',(0.,-1.,8.57182693503055E-17));
#4324=DIRECTION('ref_axis',(0.,-8.57182693503055E-17,-1.));
#4325=DIRECTION('center_axis',(0.,-1.,8.57182693503055E-17));
#4326=DIRECTION('ref_axis',(0.,-8.57182693503055E-17,-1.));
#4327=DIRECTION('axis',(0.,0.,1.));
#4328=DIRECTION('refdir',(1.,0.,0.));
#4329=DIRECTION('center_axis',(-1.,0.,0.));
#4330=DIRECTION('ref_axis',(0.,0.,-1.));
#4331=DIRECTION('',(0.,8.57182693503055E-17,-1.));
#4332=DIRECTION('',(0.,1.,8.57182693503055E-17));
#4333=DIRECTION('',(0.,8.57182693503055E-17,-1.));
#4334=DIRECTION('',(0.,1.,8.57182693503055E-17));
#4335=DIRECTION('center_axis',(0.,-8.57182693503055E-17,1.));
#4336=DIRECTION('ref_axis',(0.,1.,8.57182693503055E-17));
#4337=DIRECTION('',(-1.,0.,0.));
#4338=DIRECTION('',(0.,1.,8.57182693503055E-17));
#4339=DIRECTION('center_axis',(0.,-8.57182693503055E-17,1.));
#4340=DIRECTION('ref_axis',(0.,1.,8.57182693503055E-17));
#4341=DIRECTION('center_axis',(0.,-8.57182693503055E-17,1.));
#4342=DIRECTION('ref_axis',(0.,1.,8.57182693503055E-17));
#4343=DIRECTION('',(0.,1.,8.57182693503055E-17));
#4344=DIRECTION('',(-1.,0.,0.));
#4345=DIRECTION('',(0.,-1.,-8.57182693503055E-17));
#4346=DIRECTION('center_axis',(0.,-8.57182693503055E-17,1.));
#4347=DIRECTION('ref_axis',(0.,1.,8.57182693503055E-17));
#4348=DIRECTION('',(-1.,0.,0.));
#4349=DIRECTION('',(0.,1.,8.57182693503055E-17));
#4350=DIRECTION('center_axis',(0.,-8.57182693503055E-17,1.));
#4351=DIRECTION('ref_axis',(0.,1.,8.57182693503055E-17));
#4352=DIRECTION('center_axis',(0.,-8.57182693503055E-17,1.));
#4353=DIRECTION('ref_axis',(0.,1.,8.57182693503055E-17));
#4354=DIRECTION('',(0.,1.,8.57182693503055E-17));
#4355=DIRECTION('',(-1.,0.,0.));
#4356=DIRECTION('',(0.,-1.,-8.57182693503055E-17));
#4357=DIRECTION('center_axis',(0.,1.,8.57182693503055E-17));
#4358=DIRECTION('ref_axis',(-1.,0.,0.));
#4359=DIRECTION('center_axis',(0.,1.,8.57182693503055E-17));
#4360=DIRECTION('ref_axis',(0.,8.57182693503055E-17,-1.));
#4361=DIRECTION('',(-1.,0.,0.));
#4362=DIRECTION('center_axis',(0.,1.,8.57182693503055E-17));
#4363=DIRECTION('ref_axis',(0.,8.57182693503055E-17,-1.));
#4364=DIRECTION('',(0.,-8.57182693503055E-17,1.));
#4365=DIRECTION('center_axis',(0.,1.,8.57182693503055E-17));
#4366=DIRECTION('ref_axis',(0.,8.57182693503055E-17,-1.));
#4367=DIRECTION('',(0.,8.57182693503055E-17,-1.));
#4368=DIRECTION('center_axis',(0.,1.,8.57182693503055E-17));
#4369=DIRECTION('ref_axis',(0.,8.57182693503055E-17,-1.));
#4370=DIRECTION('',(0.,8.57182693503055E-17,-1.));
#4371=DIRECTION('center_axis',(0.,1.,8.57182693503055E-17));
#4372=DIRECTION('ref_axis',(0.,8.57182693503055E-17,-1.));
#4373=DIRECTION('',(-1.,0.,0.));
#4374=DIRECTION('center_axis',(0.,1.,8.57182693503055E-17));
#4375=DIRECTION('ref_axis',(0.,8.57182693503055E-17,-1.));
#4376=DIRECTION('center_axis',(0.,1.,8.57182693503055E-17));
#4377=DIRECTION('ref_axis',(0.,8.57182693503055E-17,-1.));
#4378=DIRECTION('center_axis',(0.,1.,8.57182693503055E-17));
#4379=DIRECTION('ref_axis',(0.,8.57182693503055E-17,-1.));
#4380=DIRECTION('center_axis',(0.,1.,8.57182693503055E-17));
#4381=DIRECTION('ref_axis',(-1.,0.,0.));
#4382=DIRECTION('',(-1.,0.,0.));
#4383=DIRECTION('center_axis',(0.,1.,8.57182693503055E-17));
#4384=DIRECTION('ref_axis',(0.,8.57182693503055E-17,-1.));
#4385=DIRECTION('center_axis',(0.,1.,8.57182693503055E-17));
#4386=DIRECTION('ref_axis',(0.,8.57182693503055E-17,-1.));
#4387=DIRECTION('',(-1.,0.,0.));
#4388=DIRECTION('center_axis',(0.,1.,8.57182693503055E-17));
#4389=DIRECTION('ref_axis',(0.,8.57182693503055E-17,-1.));
#4390=DIRECTION('',(0.,8.57182693503055E-17,-1.));
#4391=DIRECTION('center_axis',(0.,1.,8.57182693503055E-17));
#4392=DIRECTION('ref_axis',(0.,8.57182693503055E-17,-1.));
#4393=DIRECTION('',(0.,8.57182693503055E-17,-1.));
#4394=DIRECTION('center_axis',(0.,1.,8.57182693503055E-17));
#4395=DIRECTION('ref_axis',(0.,8.57182693503055E-17,-1.));
#4396=DIRECTION('',(0.,-8.57182693503055E-17,1.));
#4397=DIRECTION('center_axis',(0.,1.,8.57182693503055E-17));
#4398=DIRECTION('ref_axis',(0.,8.57182693503055E-17,-1.));
#4399=DIRECTION('center_axis',(0.,1.,8.57182693503055E-17));
#4400=DIRECTION('ref_axis',(0.,8.57182693503055E-17,-1.));
#4401=DIRECTION('center_axis',(0.,1.,8.57182693503055E-17));
#4402=DIRECTION('ref_axis',(0.,8.57182693503055E-17,-1.));
#4403=DIRECTION('center_axis',(0.,-1.,-8.57182693503055E-17));
#4404=DIRECTION('ref_axis',(0.,-8.57182693503055E-17,1.));
#4405=DIRECTION('',(0.,-1.,-8.57182693503055E-17));
#4406=DIRECTION('center_axis',(0.,-1.,-8.57182693503055E-17));
#4407=DIRECTION('ref_axis',(0.,-8.57182693503055E-17,1.));
#4408=DIRECTION('',(0.,-1.,-8.57182693503055E-17));
#4409=DIRECTION('center_axis',(-1.,0.,0.));
#4410=DIRECTION('ref_axis',(0.,0.,-1.));
#4411=DIRECTION('center_axis',(0.,-8.57182693503055E-17,1.));
#4412=DIRECTION('ref_axis',(0.,1.,8.57182693503055E-17));
#4413=DIRECTION('',(0.,-8.57182693503055E-17,1.));
#4414=DIRECTION('center_axis',(0.,8.57182693503055E-17,-1.));
#4415=DIRECTION('ref_axis',(0.,-1.,-8.57182693503055E-17));
#4416=DIRECTION('',(0.,1.,8.57182693503055E-17));
#4417=DIRECTION('',(0.,1.,8.57182693503055E-17));
#4418=DIRECTION('center_axis',(-1.,0.,0.));
#4419=DIRECTION('ref_axis',(0.,0.,-1.));
#4420=DIRECTION('',(0.,1.,8.57182693503055E-17));
#4421=DIRECTION('',(0.,1.,8.57182693503055E-17));
#4422=DIRECTION('center_axis',(0.,8.57182693503055E-17,-1.));
#4423=DIRECTION('ref_axis',(0.,-1.,-8.57182693503055E-17));
#4424=DIRECTION('',(0.,1.,8.57182693503055E-17));
#4425=DIRECTION('',(0.,1.,8.57182693503055E-17));
#4426=DIRECTION('center_axis',(1.,0.,0.));
#4427=DIRECTION('ref_axis',(0.,0.,1.));
#4428=DIRECTION('',(0.,1.,8.57182693503055E-17));
#4429=DIRECTION('',(0.,1.,8.57182693503055E-17));
#4430=DIRECTION('center_axis',(0.,-1.,-8.57182693503055E-17));
#4431=DIRECTION('ref_axis',(0.,-8.57182693503055E-17,1.));
#4432=DIRECTION('center_axis',(0.,1.,8.57182693503055E-17));
#4433=DIRECTION('ref_axis',(0.,8.57182693503055E-17,-1.));
#4434=DIRECTION('center_axis',(0.,1.,8.57182693503055E-17));
#4435=DIRECTION('ref_axis',(0.,8.57182693503055E-17,-1.));
#4436=DIRECTION('center_axis',(0.,1.,8.57182693503055E-17));
#4437=DIRECTION('ref_axis',(0.,8.57182693503055E-17,-1.));
#4438=DIRECTION('center_axis',(0.,1.,8.57182693503055E-17));
#4439=DIRECTION('ref_axis',(0.,8.57182693503055E-17,-1.));
#4440=DIRECTION('center_axis',(0.,1.,8.57182693503055E-17));
#4441=DIRECTION('ref_axis',(0.,8.57182693503055E-17,-1.));
#4442=DIRECTION('axis',(0.,0.,1.));
#4443=DIRECTION('refdir',(1.,0.,0.));
#4444=DIRECTION('axis',(0.,0.,1.));
#4445=DIRECTION('refdir',(1.,0.,0.));
#4446=DIRECTION('center_axis',(0.,-1.,8.57182693503055E-17));
#4447=DIRECTION('ref_axis',(0.,-8.57182693503055E-17,-1.));
#4448=DIRECTION('',(0.,-8.57182693503055E-17,-1.));
#4449=DIRECTION('',(-1.,0.,0.));
#4450=DIRECTION('',(0.,-8.57182693503055E-17,-1.));
#4451=DIRECTION('',(-1.,0.,0.));
#4452=DIRECTION('center_axis',(0.,0.,1.));
#4453=DIRECTION('ref_axis',(-1.,0.,0.));
#4454=DIRECTION('',(0.,-1.,0.));
#4455=DIRECTION('',(-1.,0.,0.));
#4456=DIRECTION('',(0.,-1.,0.));
#4457=DIRECTION('',(-1.,0.,0.));
#4458=DIRECTION('center_axis',(0.,-1.,6.42887020127291E-17));
#4459=DIRECTION('ref_axis',(0.,-6.42887020127291E-17,-1.));
#4460=DIRECTION('',(0.,-6.42887020127291E-17,-1.));
#4461=DIRECTION('',(-1.,0.,0.));
#4462=DIRECTION('',(0.,-6.42887020127291E-17,-1.));
#4463=DIRECTION('',(-1.,0.,0.));
#4464=DIRECTION('center_axis',(0.,1.,-6.42887020127291E-17));
#4465=DIRECTION('ref_axis',(0.,-6.42887020127291E-17,-1.));
#4466=DIRECTION('center_axis',(0.,1.,-6.42887020127291E-17));
#4467=DIRECTION('ref_axis',(0.,-6.42887020127291E-17,-1.));
#4468=DIRECTION('center_axis',(0.,0.,1.));
#4469=DIRECTION('ref_axis',(-1.,0.,0.));
#4470=DIRECTION('',(0.,-1.,0.));
#4471=DIRECTION('',(-1.,0.,0.));
#4472=DIRECTION('',(0.,-1.,0.));
#4473=DIRECTION('',(-1.,0.,0.));
#4474=DIRECTION('center_axis',(-1.,0.,0.));
#4475=DIRECTION('ref_axis',(0.,0.,-1.));
#4476=DIRECTION('center_axis',(-1.,0.,0.));
#4477=DIRECTION('ref_axis',(0.,0.,1.));
#4478=DIRECTION('',(-1.,0.,0.));
#4479=DIRECTION('center_axis',(-1.,0.,0.));
#4480=DIRECTION('ref_axis',(0.,0.,1.));
#4481=DIRECTION('center_axis',(0.,-1.,8.57182693503055E-17));
#4482=DIRECTION('ref_axis',(0.,-8.57182693503055E-17,-1.));
#4483=DIRECTION('',(0.,-8.57182693503055E-17,-1.));
#4484=DIRECTION('',(-1.,0.,0.));
#4485=DIRECTION('',(0.,-8.57182693503055E-17,-1.));
#4486=DIRECTION('',(-1.,0.,0.));
#4487=DIRECTION('center_axis',(-1.,0.,0.));
#4488=DIRECTION('ref_axis',(0.,0.,-1.));
#4489=DIRECTION('center_axis',(-1.,0.,0.));
#4490=DIRECTION('ref_axis',(0.,0.,1.));
#4491=DIRECTION('',(-1.,0.,0.));
#4492=DIRECTION('center_axis',(-1.,0.,0.));
#4493=DIRECTION('ref_axis',(0.,0.,1.));
#4494=DIRECTION('center_axis',(1.,0.,0.));
#4495=DIRECTION('ref_axis',(0.,-1.,0.));
#4496=DIRECTION('',(0.,-8.57182693503055E-17,-1.));
#4497=DIRECTION('center_axis',(-1.,0.,0.));
#4498=DIRECTION('ref_axis',(0.,0.,1.));
#4499=DIRECTION('center_axis',(-1.,0.,0.));
#4500=DIRECTION('ref_axis',(0.,0.,1.));
#4501=DIRECTION('center_axis',(-1.,0.,0.));
#4502=DIRECTION('ref_axis',(0.,0.,1.));
#4503=DIRECTION('center_axis',(-1.,0.,0.));
#4504=DIRECTION('ref_axis',(0.,0.,1.));
#4505=DIRECTION('center_axis',(-1.,0.,0.));
#4506=DIRECTION('ref_axis',(0.,0.,1.));
#4507=DIRECTION('center_axis',(-1.,0.,0.));
#4508=DIRECTION('ref_axis',(0.,0.,1.));
#4509=DIRECTION('center_axis',(-1.,0.,0.));
#4510=DIRECTION('ref_axis',(0.,0.,1.));
#4511=DIRECTION('center_axis',(-1.,0.,0.));
#4512=DIRECTION('ref_axis',(0.,0.,1.));
#4513=DIRECTION('center_axis',(1.,0.,0.));
#4514=DIRECTION('ref_axis',(0.,-1.,0.));
#4515=DIRECTION('center_axis',(1.,0.,0.));
#4516=DIRECTION('ref_axis',(0.,-1.,0.));
#4517=DIRECTION('center_axis',(1.,0.,0.));
#4518=DIRECTION('ref_axis',(0.,-1.,0.));
#4519=DIRECTION('center_axis',(-1.,0.,0.));
#4520=DIRECTION('ref_axis',(0.,0.,1.));
#4521=DIRECTION('center_axis',(-1.,0.,0.));
#4522=DIRECTION('ref_axis',(0.,0.,1.));
#4523=DIRECTION('center_axis',(-1.,0.,0.));
#4524=DIRECTION('ref_axis',(0.,0.,1.));
#4525=DIRECTION('center_axis',(-1.,0.,0.));
#4526=DIRECTION('ref_axis',(0.,0.,1.));
#4527=DIRECTION('center_axis',(-1.,0.,0.));
#4528=DIRECTION('ref_axis',(0.,0.,1.));
#4529=DIRECTION('center_axis',(-1.,0.,0.));
#4530=DIRECTION('ref_axis',(0.,0.,1.));
#4531=DIRECTION('',(0.,-8.57182693503055E-17,-1.));
#4532=DIRECTION('center_axis',(-1.,0.,0.));
#4533=DIRECTION('ref_axis',(0.,0.,1.));
#4534=DIRECTION('center_axis',(-1.,0.,0.));
#4535=DIRECTION('ref_axis',(0.,0.,1.));
#4536=DIRECTION('center_axis',(-1.,0.,0.));
#4537=DIRECTION('ref_axis',(0.,0.,-1.));
#4538=DIRECTION('center_axis',(1.,0.,0.));
#4539=DIRECTION('ref_axis',(0.,0.,1.));
#4540=DIRECTION('center_axis',(-1.,0.,0.));
#4541=DIRECTION('ref_axis',(0.,0.,-1.));
#4542=DIRECTION('center_axis',(1.,0.,0.));
#4543=DIRECTION('ref_axis',(0.,0.,1.));
#4544=DIRECTION('center_axis',(0.,-1.,8.57182693503055E-17));
#4545=DIRECTION('ref_axis',(-1.,0.,0.));
#4546=DIRECTION('',(-1.,0.,0.));
#4547=DIRECTION('center_axis',(0.,1.,-8.57182693503055E-17));
#4548=DIRECTION('ref_axis',(0.,-8.57182693503055E-17,-1.));
#4549=DIRECTION('',(-1.,0.,0.));
#4550=DIRECTION('',(-1.,0.,0.));
#4551=DIRECTION('center_axis',(0.,1.,-8.57182693503055E-17));
#4552=DIRECTION('ref_axis',(0.,-8.57182693503055E-17,-1.));
#4553=DIRECTION('center_axis',(0.,1.,-8.57182693503055E-17));
#4554=DIRECTION('ref_axis',(0.,-8.57182693503055E-17,-1.));
#4555=DIRECTION('',(-1.,0.,0.));
#4556=DIRECTION('center_axis',(0.,-1.,8.57182693503055E-17));
#4557=DIRECTION('ref_axis',(0.,-8.57182693503055E-17,-1.));
#4558=DIRECTION('',(0.,-1.,8.57182693503055E-17));
#4559=DIRECTION('center_axis',(0.,-1.,8.57182693503055E-17));
#4560=DIRECTION('ref_axis',(0.,-8.57182693503055E-17,-1.));
#4561=DIRECTION('',(0.,-1.,8.57182693503055E-17));
#4562=DIRECTION('center_axis',(1.,0.,0.));
#4563=DIRECTION('ref_axis',(0.,0.,1.));
#4564=DIRECTION('',(-1.,0.,0.));
#4565=DIRECTION('center_axis',(-1.,0.,0.));
#4566=DIRECTION('ref_axis',(0.,0.,-1.));
#4567=DIRECTION('center_axis',(-1.,0.,0.));
#4568=DIRECTION('ref_axis',(0.,0.,-1.));
#4569=DIRECTION('',(-1.,0.,0.));
#4570=DIRECTION('center_axis',(1.,0.,0.));
#4571=DIRECTION('ref_axis',(0.,0.,1.));
#4572=DIRECTION('axis',(0.,0.,1.));
#4573=DIRECTION('refdir',(1.,0.,0.));
#4574=DIRECTION('center_axis',(0.,-1.,8.57182693503055E-17));
#4575=DIRECTION('ref_axis',(0.,-8.57182693503055E-17,-1.));
#4576=DIRECTION('',(0.,-8.57182693503055E-17,-1.));
#4577=DIRECTION('',(1.,0.,0.));
#4578=DIRECTION('',(0.,-8.57182693503055E-17,-1.));
#4579=DIRECTION('',(1.,0.,0.));
#4580=DIRECTION('center_axis',(0.,0.,1.));
#4581=DIRECTION('ref_axis',(1.,0.,0.));
#4582=DIRECTION('',(0.,-1.,0.));
#4583=DIRECTION('',(1.,0.,0.));
#4584=DIRECTION('',(0.,-1.,0.));
#4585=DIRECTION('',(1.,0.,0.));
#4586=DIRECTION('center_axis',(0.,-1.,6.42887020127291E-17));
#4587=DIRECTION('ref_axis',(0.,-6.42887020127291E-17,-1.));
#4588=DIRECTION('',(0.,-6.42887020127291E-17,-1.));
#4589=DIRECTION('',(1.,0.,0.));
#4590=DIRECTION('',(0.,-6.42887020127291E-17,-1.));
#4591=DIRECTION('',(1.,0.,0.));
#4592=DIRECTION('center_axis',(0.,-1.,6.42887020127291E-17));
#4593=DIRECTION('ref_axis',(0.,-6.42887020127291E-17,-1.));
#4594=DIRECTION('center_axis',(0.,-1.,6.42887020127291E-17));
#4595=DIRECTION('ref_axis',(0.,-6.42887020127291E-17,-1.));
#4596=DIRECTION('center_axis',(0.,0.,1.));
#4597=DIRECTION('ref_axis',(1.,0.,0.));
#4598=DIRECTION('',(0.,-1.,0.));
#4599=DIRECTION('',(1.,0.,0.));
#4600=DIRECTION('',(0.,-1.,0.));
#4601=DIRECTION('',(1.,0.,0.));
#4602=DIRECTION('center_axis',(1.,0.,0.));
#4603=DIRECTION('ref_axis',(0.,0.,-1.));
#4604=DIRECTION('center_axis',(-1.,0.,0.));
#4605=DIRECTION('ref_axis',(0.,0.,1.));
#4606=DIRECTION('',(1.,0.,0.));
#4607=DIRECTION('center_axis',(-1.,0.,0.));
#4608=DIRECTION('ref_axis',(0.,0.,1.));
#4609=DIRECTION('center_axis',(0.,-1.,8.57182693503055E-17));
#4610=DIRECTION('ref_axis',(0.,-8.57182693503055E-17,-1.));
#4611=DIRECTION('',(0.,-8.57182693503055E-17,-1.));
#4612=DIRECTION('',(1.,0.,0.));
#4613=DIRECTION('',(0.,-8.57182693503055E-17,-1.));
#4614=DIRECTION('',(1.,0.,0.));
#4615=DIRECTION('center_axis',(1.,0.,0.));
#4616=DIRECTION('ref_axis',(0.,0.,-1.));
#4617=DIRECTION('center_axis',(-1.,0.,0.));
#4618=DIRECTION('ref_axis',(0.,0.,1.));
#4619=DIRECTION('',(1.,0.,0.));
#4620=DIRECTION('center_axis',(-1.,0.,0.));
#4621=DIRECTION('ref_axis',(0.,0.,1.));
#4622=DIRECTION('center_axis',(-1.,0.,0.));
#4623=DIRECTION('ref_axis',(0.,-1.,0.));
#4624=DIRECTION('',(0.,-8.57182693503055E-17,-1.));
#4625=DIRECTION('center_axis',(-1.,0.,0.));
#4626=DIRECTION('ref_axis',(0.,0.,1.));
#4627=DIRECTION('center_axis',(-1.,0.,0.));
#4628=DIRECTION('ref_axis',(0.,0.,1.));
#4629=DIRECTION('center_axis',(-1.,0.,0.));
#4630=DIRECTION('ref_axis',(0.,0.,1.));
#4631=DIRECTION('center_axis',(-1.,0.,0.));
#4632=DIRECTION('ref_axis',(0.,0.,1.));
#4633=DIRECTION('center_axis',(-1.,0.,0.));
#4634=DIRECTION('ref_axis',(0.,0.,1.));
#4635=DIRECTION('center_axis',(-1.,0.,0.));
#4636=DIRECTION('ref_axis',(0.,0.,1.));
#4637=DIRECTION('center_axis',(-1.,0.,0.));
#4638=DIRECTION('ref_axis',(0.,0.,1.));
#4639=DIRECTION('center_axis',(-1.,0.,0.));
#4640=DIRECTION('ref_axis',(0.,0.,1.));
#4641=DIRECTION('center_axis',(-1.,0.,0.));
#4642=DIRECTION('ref_axis',(0.,-1.,0.));
#4643=DIRECTION('center_axis',(-1.,0.,0.));
#4644=DIRECTION('ref_axis',(0.,-1.,0.));
#4645=DIRECTION('center_axis',(-1.,0.,0.));
#4646=DIRECTION('ref_axis',(0.,-1.,0.));
#4647=DIRECTION('center_axis',(-1.,0.,0.));
#4648=DIRECTION('ref_axis',(0.,0.,1.));
#4649=DIRECTION('center_axis',(-1.,0.,0.));
#4650=DIRECTION('ref_axis',(0.,0.,1.));
#4651=DIRECTION('',(0.,-8.57182693503055E-17,-1.));
#4652=DIRECTION('center_axis',(-1.,0.,0.));
#4653=DIRECTION('ref_axis',(0.,0.,1.));
#4654=DIRECTION('center_axis',(-1.,0.,0.));
#4655=DIRECTION('ref_axis',(0.,0.,1.));
#4656=DIRECTION('center_axis',(-1.,0.,0.));
#4657=DIRECTION('ref_axis',(0.,0.,1.));
#4658=DIRECTION('center_axis',(-1.,0.,0.));
#4659=DIRECTION('ref_axis',(0.,0.,1.));
#4660=DIRECTION('center_axis',(-1.,0.,0.));
#4661=DIRECTION('ref_axis',(0.,0.,1.));
#4662=DIRECTION('center_axis',(-1.,0.,0.));
#4663=DIRECTION('ref_axis',(0.,0.,1.));
#4664=DIRECTION('center_axis',(1.,0.,0.));
#4665=DIRECTION('ref_axis',(0.,0.,-1.));
#4666=DIRECTION('center_axis',(-1.,0.,0.));
#4667=DIRECTION('ref_axis',(0.,0.,1.));
#4668=DIRECTION('center_axis',(1.,0.,0.));
#4669=DIRECTION('ref_axis',(0.,0.,-1.));
#4670=DIRECTION('center_axis',(-1.,0.,0.));
#4671=DIRECTION('ref_axis',(0.,0.,1.));
#4672=DIRECTION('center_axis',(0.,-1.,8.57182693503055E-17));
#4673=DIRECTION('ref_axis',(1.,0.,0.));
#4674=DIRECTION('',(1.,0.,0.));
#4675=DIRECTION('center_axis',(0.,-1.,8.57182693503055E-17));
#4676=DIRECTION('ref_axis',(0.,-8.57182693503055E-17,-1.));
#4677=DIRECTION('center_axis',(0.,-1.,8.57182693503055E-17));
#4678=DIRECTION('ref_axis',(0.,-8.57182693503055E-17,-1.));
#4679=DIRECTION('',(1.,0.,0.));
#4680=DIRECTION('',(1.,0.,0.));
#4681=DIRECTION('center_axis',(0.,-1.,8.57182693503055E-17));
#4682=DIRECTION('ref_axis',(0.,-8.57182693503055E-17,-1.));
#4683=DIRECTION('',(1.,0.,0.));
#4684=DIRECTION('center_axis',(0.,-1.,8.57182693503055E-17));
#4685=DIRECTION('ref_axis',(0.,-8.57182693503055E-17,-1.));
#4686=DIRECTION('',(0.,-1.,8.57182693503055E-17));
#4687=DIRECTION('center_axis',(0.,-1.,8.57182693503055E-17));
#4688=DIRECTION('ref_axis',(0.,-8.57182693503055E-17,-1.));
#4689=DIRECTION('',(0.,-1.,8.57182693503055E-17));
#4690=DIRECTION('center_axis',(-1.,0.,0.));
#4691=DIRECTION('ref_axis',(0.,0.,1.));
#4692=DIRECTION('',(1.,0.,0.));
#4693=DIRECTION('center_axis',(1.,0.,0.));
#4694=DIRECTION('ref_axis',(0.,0.,-1.));
#4695=DIRECTION('center_axis',(1.,0.,0.));
#4696=DIRECTION('ref_axis',(0.,0.,-1.));
#4697=DIRECTION('',(1.,0.,0.));
#4698=DIRECTION('center_axis',(-1.,0.,0.));
#4699=DIRECTION('ref_axis',(0.,0.,1.));
#4700=DIRECTION('axis',(0.,0.,1.));
#4701=DIRECTION('refdir',(1.,0.,0.));
#4702=DIRECTION('center_axis',(0.,0.,-1.));
#4703=DIRECTION('ref_axis',(-1.,0.,0.));
#4704=DIRECTION('center_axis',(0.,0.,1.));
#4705=DIRECTION('ref_axis',(1.,0.,0.));
#4706=DIRECTION('',(0.,0.,1.));
#4707=DIRECTION('center_axis',(0.,0.,1.));
#4708=DIRECTION('ref_axis',(1.,0.,0.));
#4709=DIRECTION('center_axis',(0.,0.,1.));
#4710=DIRECTION('ref_axis',(1.,0.,0.));
#4711=DIRECTION('center_axis',(0.,0.,1.));
#4712=DIRECTION('ref_axis',(1.,0.,0.));
#4713=DIRECTION('center_axis',(0.,0.,1.));
#4714=DIRECTION('ref_axis',(1.,0.,0.));
#4715=DIRECTION('center_axis',(0.,0.,1.));
#4716=DIRECTION('ref_axis',(1.,0.,0.));
#4717=DIRECTION('center_axis',(0.,0.,1.));
#4718=DIRECTION('ref_axis',(1.,0.,0.));
#4719=DIRECTION('center_axis',(0.,0.,1.));
#4720=DIRECTION('ref_axis',(1.,0.,0.));
#4721=DIRECTION('center_axis',(0.,0.,1.));
#4722=DIRECTION('ref_axis',(1.,0.,0.));
#4723=DIRECTION('center_axis',(1.22464679914735E-16,-1.,0.));
#4724=DIRECTION('ref_axis',(-1.,-1.22464679914735E-16,0.));
#4725=DIRECTION('center_axis',(0.,0.,1.));
#4726=DIRECTION('ref_axis',(1.,0.,0.));
#4727=DIRECTION('center_axis',(1.22464679914735E-16,-1.,0.));
#4728=DIRECTION('ref_axis',(-1.,-1.22464679914735E-16,0.));
#4729=DIRECTION('axis',(0.,0.,1.));
#4730=DIRECTION('refdir',(1.,0.,0.));
#4731=DIRECTION('axis',(0.,0.,1.));
#4732=DIRECTION('refdir',(1.,0.,0.));
#4733=DIRECTION('axis',(0.,0.,1.));
#4734=DIRECTION('refdir',(1.,0.,0.));
#4735=DIRECTION('axis',(0.,0.,1.));
#4736=DIRECTION('refdir',(1.,0.,0.));
#4737=DIRECTION('axis',(0.,0.,1.));
#4738=DIRECTION('refdir',(1.,0.,0.));
#4739=DIRECTION('axis',(0.,0.,1.));
#4740=DIRECTION('refdir',(1.,0.,0.));
#4741=DIRECTION('axis',(0.,0.,1.));
#4742=DIRECTION('refdir',(1.,0.,0.));
#4743=DIRECTION('axis',(0.,0.,1.));
#4744=DIRECTION('refdir',(1.,0.,0.));
#4745=DIRECTION('axis',(0.,0.,1.));
#4746=DIRECTION('refdir',(1.,0.,0.));
#4747=DIRECTION('axis',(0.,0.,1.));
#4748=DIRECTION('refdir',(1.,0.,0.));
#4749=DIRECTION('axis',(0.,0.,1.));
#4750=DIRECTION('refdir',(1.,0.,0.));
#4751=DIRECTION('axis',(0.,0.,1.));
#4752=DIRECTION('refdir',(1.,0.,0.));
#4753=DIRECTION('center_axis',(0.,-1.,0.));
#4754=DIRECTION('ref_axis',(0.,0.,-1.));
#4755=DIRECTION('center_axis',(0.,1.,0.));
#4756=DIRECTION('ref_axis',(0.,0.,-1.));
#4757=DIRECTION('',(-8.65956056235503E-17,-0.70710678118654,0.707106781186555));
#4758=DIRECTION('center_axis',(0.,-1.,0.));
#4759=DIRECTION('ref_axis',(0.,0.,-1.));
#4760=DIRECTION('center_axis',(0.,1.,0.));
#4761=DIRECTION('ref_axis',(0.,0.,-1.));
#4762=DIRECTION('center_axis',(0.,-1.,0.));
#4763=DIRECTION('ref_axis',(0.,0.,-1.));
#4764=DIRECTION('center_axis',(0.,1.,0.));
#4765=DIRECTION('ref_axis',(0.,0.,-1.));
#4766=DIRECTION('center_axis',(0.,1.,0.));
#4767=DIRECTION('ref_axis',(0.,0.,1.));
#4768=DIRECTION('',(0.,1.,0.));
#4769=DIRECTION('center_axis',(0.,1.,0.));
#4770=DIRECTION('ref_axis',(1.,0.,0.));
#4771=DIRECTION('center_axis',(0.,1.,0.));
#4772=DIRECTION('ref_axis',(0.,0.,-1.));
#4773=DIRECTION('center_axis',(0.,-1.,0.));
#4774=DIRECTION('ref_axis',(0.,0.,-1.));
#4775=DIRECTION('',(-8.65956056235493E-17,-0.707106781186548,-0.707106781186547));
#4776=DIRECTION('center_axis',(0.,-1.,0.));
#4777=DIRECTION('ref_axis',(0.,0.,-1.));
#4778=DIRECTION('center_axis',(0.,1.,0.));
#4779=DIRECTION('ref_axis',(0.,0.,1.));
#4780=DIRECTION('center_axis',(0.,1.,0.));
#4781=DIRECTION('ref_axis',(1.,0.,0.));
#4782=DIRECTION('',(0.,-1.,0.));
#4783=DIRECTION('center_axis',(0.,1.,0.));
#4784=DIRECTION('ref_axis',(0.,0.,-1.));
#4785=DIRECTION('center_axis',(0.,-1.,0.));
#4786=DIRECTION('ref_axis',(0.,0.,-1.));
#4787=DIRECTION('',(8.65956056235503E-17,0.70710678118654,0.707106781186555));
#4788=DIRECTION('center_axis',(0.,1.,0.));
#4789=DIRECTION('ref_axis',(0.,0.,-1.));
#4790=DIRECTION('center_axis',(0.,-1.,0.));
#4791=DIRECTION('ref_axis',(0.,0.,-1.));
#4792=DIRECTION('center_axis',(0.,1.,0.));
#4793=DIRECTION('ref_axis',(1.,0.,0.));
#4794=DIRECTION('center_axis',(0.,-1.,0.));
#4795=DIRECTION('ref_axis',(0.,0.,-1.));
#4796=DIRECTION('center_axis',(0.,1.,0.));
#4797=DIRECTION('ref_axis',(0.,0.,1.));
#4798=DIRECTION('center_axis',(0.,1.,0.));
#4799=DIRECTION('ref_axis',(1.,0.,0.));
#4800=DIRECTION('',(0.,1.,0.));
#4801=DIRECTION('center_axis',(0.,-1.,0.));
#4802=DIRECTION('ref_axis',(0.,0.,-1.));
#4803=DIRECTION('center_axis',(0.,1.,0.));
#4804=DIRECTION('ref_axis',(0.,0.,-1.));
#4805=DIRECTION('',(8.65956056235493E-17,0.707106781186548,-0.707106781186547));
#4806=DIRECTION('center_axis',(0.,1.,0.));
#4807=DIRECTION('ref_axis',(0.,0.,-1.));
#4808=DIRECTION('center_axis',(0.,1.,0.));
#4809=DIRECTION('ref_axis',(0.,0.,1.));
#4810=DIRECTION('',(0.,-1.,0.));
#4811=DIRECTION('center_axis',(0.,1.,0.));
#4812=DIRECTION('ref_axis',(1.,0.,0.));
#4813=DIRECTION('center_axis',(0.,-1.,0.));
#4814=DIRECTION('ref_axis',(0.,0.,-1.));
#4815=DIRECTION('center_axis',(0.,1.,0.));
#4816=DIRECTION('ref_axis',(1.,0.,0.));
#4817=DIRECTION('center_axis',(0.,1.,0.));
#4818=DIRECTION('ref_axis',(0.,0.,1.));
#4819=DIRECTION('center_axis',(0.,1.,0.));
#4820=DIRECTION('ref_axis',(1.,0.,0.));
#4821=DIRECTION('',(0.,1.,0.));
#4822=DIRECTION('center_axis',(0.,1.,0.));
#4823=DIRECTION('ref_axis',(1.,0.,0.));
#4824=DIRECTION('center_axis',(0.,1.,0.));
#4825=DIRECTION('ref_axis',(1.,0.,0.));
#4826=DIRECTION('center_axis',(0.,1.,0.));
#4827=DIRECTION('ref_axis',(0.,0.,1.));
#4828=DIRECTION('center_axis',(0.,1.,0.));
#4829=DIRECTION('ref_axis',(1.,0.,0.));
#4830=DIRECTION('',(0.,1.,0.));
#4831=DIRECTION('center_axis',(0.,1.,0.));
#4832=DIRECTION('ref_axis',(0.,0.,1.));
#4833=DIRECTION('center_axis',(0.,1.,0.));
#4834=DIRECTION('ref_axis',(1.,0.,0.));
#4835=DIRECTION('',(-1.93482561475974E-17,0.987440631916705,-0.157990501106673));
#4836=DIRECTION('center_axis',(0.,1.,0.));
#4837=DIRECTION('ref_axis',(0.,0.,1.));
#4838=DIRECTION('center_axis',(0.,1.,0.));
#4839=DIRECTION('ref_axis',(1.,0.,0.));
#4840=DIRECTION('',(0.,1.,0.));
#4841=DIRECTION('center_axis',(0.,-1.,0.));
#4842=DIRECTION('ref_axis',(0.,0.,1.));
#4843=DIRECTION('',(1.93482561475974E-17,-0.987440631916705,-0.157990501106673));
#4844=DIRECTION('center_axis',(0.,1.,0.));
#4845=DIRECTION('ref_axis',(1.,0.,0.));
#4846=DIRECTION('center_axis',(0.,1.,0.));
#4847=DIRECTION('ref_axis',(0.,0.,1.));
#4848=DIRECTION('center_axis',(0.,1.,0.));
#4849=DIRECTION('ref_axis',(1.,0.,0.));
#4850=DIRECTION('',(0.,1.,0.));
#4851=DIRECTION('center_axis',(0.,-1.,0.));
#4852=DIRECTION('ref_axis',(0.,0.,-1.));
#4853=DIRECTION('center_axis',(0.,1.,0.));
#4854=DIRECTION('ref_axis',(1.,0.,0.));
#4855=DIRECTION('center_axis',(0.,1.,0.));
#4856=DIRECTION('ref_axis',(0.,0.,1.));
#4857=DIRECTION('center_axis',(0.,1.,0.));
#4858=DIRECTION('ref_axis',(1.,0.,0.));
#4859=DIRECTION('',(0.,1.,0.));
#4860=DIRECTION('center_axis',(0.,1.,0.));
#4861=DIRECTION('ref_axis',(1.,0.,0.));
#4862=DIRECTION('center_axis',(0.,1.,0.));
#4863=DIRECTION('ref_axis',(1.,0.,0.));
#4864=DIRECTION('center_axis',(0.,1.,0.));
#4865=DIRECTION('ref_axis',(1.,0.,0.));
#4866=DIRECTION('center_axis',(0.,1.,0.));
#4867=DIRECTION('ref_axis',(0.,0.,1.));
#4868=DIRECTION('center_axis',(0.,1.,0.));
#4869=DIRECTION('ref_axis',(1.,0.,0.));
#4870=DIRECTION('',(0.,-1.,0.));
#4871=DIRECTION('center_axis',(0.,-1.,0.));
#4872=DIRECTION('ref_axis',(0.,0.,-1.));
#4873=DIRECTION('center_axis',(0.,1.,0.));
#4874=DIRECTION('ref_axis',(1.,0.,0.));
#4875=DIRECTION('center_axis',(0.,1.,0.));
#4876=DIRECTION('ref_axis',(0.,0.,1.));
#4877=DIRECTION('center_axis',(0.,1.,0.));
#4878=DIRECTION('ref_axis',(1.,0.,0.));
#4879=DIRECTION('',(0.,-1.,0.));
#4880=DIRECTION('center_axis',(0.,1.,0.));
#4881=DIRECTION('ref_axis',(1.,0.,0.));
#4882=DIRECTION('center_axis',(0.,1.,0.));
#4883=DIRECTION('ref_axis',(1.,0.,0.));
#4884=DIRECTION('center_axis',(0.,1.,0.));
#4885=DIRECTION('ref_axis',(0.,0.,1.));
#4886=DIRECTION('center_axis',(0.,1.,0.));
#4887=DIRECTION('ref_axis',(1.,0.,0.));
#4888=DIRECTION('',(0.,-1.,0.));
#4889=DIRECTION('center_axis',(0.,-1.,0.));
#4890=DIRECTION('ref_axis',(0.,0.,-1.));
#4891=DIRECTION('axis',(0.,0.,1.));
#4892=DIRECTION('refdir',(1.,0.,0.));
#4893=DIRECTION('center_axis',(0.,-1.,0.));
#4894=DIRECTION('ref_axis',(1.,0.,0.));
#4895=DIRECTION('center_axis',(0.,1.,0.));
#4896=DIRECTION('ref_axis',(1.,0.,0.));
#4897=DIRECTION('center_axis',(0.,1.,0.));
#4898=DIRECTION('ref_axis',(1.,0.,0.));
#4899=DIRECTION('center_axis',(0.,1.,0.));
#4900=DIRECTION('ref_axis',(0.,0.,1.));
#4901=DIRECTION('',(0.,-1.,0.));
#4902=DIRECTION('center_axis',(0.,1.,0.));
#4903=DIRECTION('ref_axis',(1.,0.,0.));
#4904=DIRECTION('center_axis',(0.,1.,0.));
#4905=DIRECTION('ref_axis',(0.,0.,1.));
#4906=DIRECTION('center_axis',(0.,1.,0.));
#4907=DIRECTION('ref_axis',(1.,0.,0.));
#4908=DIRECTION('center_axis',(0.,-1.,0.));
#4909=DIRECTION('ref_axis',(0.,0.,1.));
#4910=DIRECTION('center_axis',(0.,1.,0.));
#4911=DIRECTION('ref_axis',(1.,0.,0.));
#4912=DIRECTION('',(8.65956056235493E-17,-0.707106781186548,-0.707106781186547));
#4913=DIRECTION('center_axis',(0.,1.,0.));
#4914=DIRECTION('ref_axis',(0.,0.,1.));
#4915=DIRECTION('',(0.,1.,0.));
#4916=DIRECTION('center_axis',(0.,1.,0.));
#4917=DIRECTION('ref_axis',(1.,0.,0.));
#4918=DIRECTION('center_axis',(0.,-1.,0.));
#4919=DIRECTION('ref_axis',(1.,0.,0.));
#4920=DIRECTION('center_axis',(0.,1.,0.));
#4921=DIRECTION('ref_axis',(1.,0.,0.));
#4922=DIRECTION('center_axis',(0.,-1.,0.));
#4923=DIRECTION('ref_axis',(0.,0.,1.));
#4924=DIRECTION('',(-8.65956056235493E-17,0.707106781186548,0.707106781186547));
#4925=DIRECTION('axis',(0.,0.,1.));
#4926=DIRECTION('refdir',(1.,0.,0.));
#4927=DIRECTION('center_axis',(0.,-1.,0.));
#4928=DIRECTION('ref_axis',(0.,0.,-1.));
#4929=DIRECTION('center_axis',(0.,1.,0.));
#4930=DIRECTION('ref_axis',(1.,0.,0.));
#4931=DIRECTION('center_axis',(0.,1.,0.));
#4932=DIRECTION('ref_axis',(1.,0.,0.));
#4933=DIRECTION('center_axis',(0.,1.,0.));
#4934=DIRECTION('ref_axis',(0.,0.,1.));
#4935=DIRECTION('center_axis',(0.,1.,0.));
#4936=DIRECTION('ref_axis',(1.,0.,0.));
#4937=DIRECTION('',(0.,-1.,0.));
#4938=DIRECTION('center_axis',(0.,1.,0.));
#4939=DIRECTION('ref_axis',(1.,0.,0.));
#4940=DIRECTION('center_axis',(0.,1.,0.));
#4941=DIRECTION('ref_axis',(1.,0.,0.));
#4942=DIRECTION('center_axis',(0.,1.,0.));
#4943=DIRECTION('ref_axis',(0.,0.,1.));
#4944=DIRECTION('center_axis',(0.,1.,0.));
#4945=DIRECTION('ref_axis',(1.,0.,0.));
#4946=DIRECTION('',(-8.65956056235493E-17,0.707106781186548,-0.707106781186547));
#4947=DIRECTION('center_axis',(0.,1.,0.));
#4948=DIRECTION('ref_axis',(0.,0.,1.));
#4949=DIRECTION('center_axis',(0.,1.,0.));
#4950=DIRECTION('ref_axis',(1.,0.,0.));
#4951=DIRECTION('',(0.,1.,0.));
#4952=DIRECTION('center_axis',(0.,-1.,0.));
#4953=DIRECTION('ref_axis',(0.,0.,-1.));
#4954=DIRECTION('center_axis',(0.,1.,0.));
#4955=DIRECTION('ref_axis',(1.,0.,0.));
#4956=DIRECTION('center_axis',(0.,1.,0.));
#4957=DIRECTION('ref_axis',(0.,0.,1.));
#4958=DIRECTION('',(8.65956056235493E-17,-0.707106781186548,0.707106781186547));
#4959=DIRECTION('axis',(0.,0.,1.));
#4960=DIRECTION('refdir',(1.,0.,0.));
#4961=DIRECTION('center_axis',(0.,-1.,0.));
#4962=DIRECTION('ref_axis',(1.,0.,0.));
#4963=DIRECTION('center_axis',(0.,1.,0.));
#4964=DIRECTION('ref_axis',(1.,0.,0.));
#4965=DIRECTION('center_axis',(0.,1.,0.));
#4966=DIRECTION('ref_axis',(1.,0.,0.));
#4967=DIRECTION('center_axis',(0.,1.,0.));
#4968=DIRECTION('ref_axis',(0.,0.,1.));
#4969=DIRECTION('',(0.,-1.,0.));
#4970=DIRECTION('center_axis',(0.,1.,0.));
#4971=DIRECTION('ref_axis',(1.,0.,0.));
#4972=DIRECTION('center_axis',(0.,1.,0.));
#4973=DIRECTION('ref_axis',(0.,0.,1.));
#4974=DIRECTION('center_axis',(0.,1.,0.));
#4975=DIRECTION('ref_axis',(1.,0.,0.));
#4976=DIRECTION('center_axis',(0.,1.,0.));
#4977=DIRECTION('ref_axis',(0.,0.,1.));
#4978=DIRECTION('',(0.,1.,0.));
#4979=DIRECTION('',(-6.08761714766374E-5,0.999999998147046,7.75443361893665E-20));
#4980=DIRECTION('',(0.999999998147046,6.08761714812451E-5,-1.25247034733451E-15));
#4981=DIRECTION('',(-6.0876171481578E-5,0.999999998147046,-2.57357144824417E-20));
#4982=DIRECTION('',(0.999999998147046,6.0876171481578E-5,4.44089209027163E-16));
#4983=DIRECTION('',(-6.0876171481578E-5,0.999999998147046,-2.57357144824417E-20));
#4984=DIRECTION('',(0.999999998147046,6.0876171481578E-5,4.44089209027163E-16));
#4985=DIRECTION('',(-6.0876171481578E-5,0.999999998147046,-2.57357144824417E-20));
#4986=DIRECTION('',(0.999999998147046,6.0876171481578E-5,4.44089209027163E-16));
#4987=DIRECTION('',(-6.08761714766374E-5,0.999999998147047,7.7544336187986E-20));
#4988=DIRECTION('',(0.999999998147047,6.08761714812451E-5,-1.25247034733451E-15));
#4989=DIRECTION('',(-6.0876171481578E-5,0.999999998147046,-2.57357144824417E-20));
#4990=DIRECTION('',(0.999999998147046,6.0876171481578E-5,4.44089209027163E-16));
#4991=DIRECTION('',(-6.0876171481578E-5,0.999999998147046,-2.57357144824417E-20));
#4992=DIRECTION('',(0.999999998147046,6.0876171481578E-5,4.44089209027163E-16));
#4993=DIRECTION('',(-6.0876171481578E-5,0.999999998147046,-2.57357144824417E-20));
#4994=DIRECTION('',(0.999999998147046,6.0876171481578E-5,4.44089209027163E-16));
#4995=DIRECTION('',(-6.0876171473847E-5,0.999999998147047,-2.57361970243427E-20));
#4996=DIRECTION('',(0.999999998147047,6.08761714784546E-5,4.4408920985004E-16));
#4997=DIRECTION('',(-6.0876171481578E-5,0.999999998147046,-2.57357144824417E-20));
#4998=DIRECTION('',(0.999999998147046,6.0876171481578E-5,4.44089209027163E-16));
#4999=DIRECTION('',(-6.0876171481578E-5,0.999999998147046,-2.57357144824417E-20));
#5000=DIRECTION('',(0.999999998147046,6.0876171481578E-5,4.44089209027163E-16));
#5001=DIRECTION('',(-6.0876171481578E-5,0.999999998147046,-2.57357144824417E-20));
#5002=DIRECTION('',(0.999999998147046,6.0876171481578E-5,4.44089209027163E-16));
#5003=DIRECTION('',(-6.08761714766374E-5,0.999999998147047,7.75443361864082E-20));
#5004=DIRECTION('',(0.999999998147047,6.08761714812451E-5,-1.2524703473345E-15));
#5005=DIRECTION('',(-6.0876171481578E-5,0.999999998147046,-2.57357144824417E-20));
#5006=DIRECTION('',(0.999999998147046,6.0876171481578E-5,4.44089209027163E-16));
#5007=DIRECTION('',(-6.0876171481578E-5,0.999999998147046,-2.57357144824417E-20));
#5008=DIRECTION('',(0.999999998147046,6.0876171481578E-5,4.44089209027163E-16));
#5009=DIRECTION('',(-6.0876171481578E-5,0.999999998147046,-2.57357144824417E-20));
#5010=DIRECTION('',(0.999999998147046,6.0876171481578E-5,4.44089209027163E-16));
#5011=DIRECTION('',(-6.08761714766374E-5,0.999999998147047,7.75443361844361E-20));
#5012=DIRECTION('',(0.999999998147047,6.08761714812451E-5,-1.25247034733451E-15));
#5013=DIRECTION('',(-6.0876171481578E-5,0.999999998147046,-2.57357144824417E-20));
#5014=DIRECTION('',(0.999999998147046,6.0876171481578E-5,4.44089209027163E-16));
#5015=DIRECTION('',(-6.0876171481578E-5,0.999999998147046,-2.57357144824417E-20));
#5016=DIRECTION('',(0.999999998147046,6.0876171481578E-5,4.44089209027163E-16));
#5017=DIRECTION('',(-6.0876171481578E-5,0.999999998147046,-2.57357144824417E-20));
#5018=DIRECTION('',(0.999999998147046,6.0876171481578E-5,4.44089209027163E-16));
#5019=DIRECTION('',(-6.08761714766374E-5,0.999999998147047,7.75443361856194E-20));
#5020=DIRECTION('',(0.999999998147047,6.08761714812451E-5,-1.2524703473345E-15));
#5021=DIRECTION('',(-6.0876171481578E-5,0.999999998147046,-2.57357144824417E-20));
#5022=DIRECTION('',(0.999999998147046,6.0876171481578E-5,4.44089209027163E-16));
#5023=DIRECTION('',(-6.0876171481578E-5,0.999999998147046,-2.57357144824417E-20));
#5024=DIRECTION('',(0.999999998147046,6.0876171481578E-5,4.44089209027163E-16));
#5025=DIRECTION('',(-6.0876171481578E-5,0.999999998147046,-2.57357144824417E-20));
#5026=DIRECTION('',(0.999999998147046,6.0876171481578E-5,4.44089209027163E-16));
#5027=DIRECTION('',(-6.08761714766374E-5,0.999999998147047,7.75443361848305E-20));
#5028=DIRECTION('',(0.999999998147047,6.08761714812451E-5,-1.2524703473345E-15));
#5029=DIRECTION('',(-6.0876171481578E-5,0.999999998147046,-2.57357144824417E-20));
#5030=DIRECTION('',(0.999999998147046,6.0876171481578E-5,4.44089209027163E-16));
#5031=DIRECTION('',(-6.0876171481578E-5,0.999999998147046,-2.57357144824417E-20));
#5032=DIRECTION('',(0.999999998147046,6.0876171481578E-5,4.44089209027163E-16));
#5033=DIRECTION('',(-6.0876171481578E-5,0.999999998147046,-2.57357144824417E-20));
#5034=DIRECTION('',(0.999999998147046,6.0876171481578E-5,4.44089209027163E-16));
#5035=DIRECTION('',(-6.08761714766374E-5,0.999999998147047,7.75443361844361E-20));
#5036=DIRECTION('',(0.999999998147047,6.08761714812451E-5,-1.25247034733451E-15));
#5037=DIRECTION('',(-6.0876171481578E-5,0.999999998147046,-2.57357144824417E-20));
#5038=DIRECTION('',(0.999999998147046,6.0876171481578E-5,4.44089209027163E-16));
#5039=DIRECTION('',(-6.0876171481578E-5,0.999999998147046,-2.57357144824417E-20));
#5040=DIRECTION('',(0.999999998147046,6.0876171481578E-5,4.44089209027163E-16));
#5041=DIRECTION('',(-6.0876171481578E-5,0.999999998147046,-2.57357144824417E-20));
#5042=DIRECTION('',(0.999999998147046,6.0876171481578E-5,4.44089209027163E-16));
#5043=DIRECTION('',(-6.08761714676915E-5,0.999999998147047,-2.57354074507017E-20));
#5044=DIRECTION('',(0.999999998147047,6.08761714722992E-5,4.44089209850038E-16));
#5045=DIRECTION('',(-6.0876171481578E-5,0.999999998147046,-2.57357144824417E-20));
#5046=DIRECTION('',(0.999999998147046,6.0876171481578E-5,4.44089209027163E-16));
#5047=DIRECTION('',(-6.0876171481578E-5,0.999999998147046,-2.57357144824417E-20));
#5048=DIRECTION('',(0.999999998147046,6.0876171481578E-5,4.44089209027163E-16));
#5049=DIRECTION('',(-6.0876171481578E-5,0.999999998147046,-2.57357144824417E-20));
#5050=DIRECTION('',(0.999999998147046,6.0876171481578E-5,4.44089209027163E-16));
#5051=DIRECTION('',(-6.08761714766374E-5,0.999999998147047,7.75443361848305E-20));
#5052=DIRECTION('',(0.999999998147047,6.08761714812451E-5,-1.2524703473345E-15));
#5053=DIRECTION('',(-6.0876171481578E-5,0.999999998147046,-2.57357144824417E-20));
#5054=DIRECTION('',(0.999999998147046,6.0876171481578E-5,4.44089209027163E-16));
#5055=DIRECTION('',(-6.0876171481578E-5,0.999999998147046,-2.57357144824417E-20));
#5056=DIRECTION('',(0.999999998147046,6.0876171481578E-5,4.44089209027163E-16));
#5057=DIRECTION('',(-6.0876171481578E-5,0.999999998147046,-2.57357144824417E-20));
#5058=DIRECTION('',(0.999999998147046,6.0876171481578E-5,4.44089209027163E-16));
#5059=DIRECTION('',(-6.08761714789435E-5,0.999999998147049,5.39102979701789E-17));
#5060=DIRECTION('',(0.999999998147046,6.08761714837245E-5,-1.25074841044861E-15));
#5061=DIRECTION('',(-6.0876171481578E-5,0.999999998147046,-2.57357144824417E-20));
#5062=DIRECTION('',(0.999999998147046,6.0876171481578E-5,4.44089209027163E-16));
#5063=DIRECTION('',(-6.0876171481578E-5,0.999999998147046,-2.57357144824417E-20));
#5064=DIRECTION('',(0.999999998147046,6.0876171481578E-5,4.44089209027163E-16));
#5065=DIRECTION('',(-6.0876171481578E-5,0.999999998147046,-2.57357144824417E-20));
#5066=DIRECTION('',(0.999999998147046,6.0876171481578E-5,4.44089209027163E-16));
#5067=DIRECTION('',(-6.08761714676915E-5,0.999999998147047,-2.57354085263135E-20));
#5068=DIRECTION('',(0.999999998147047,6.08761714722992E-5,4.44089209850037E-16));
#5069=DIRECTION('',(-6.0876171481578E-5,0.999999998147046,-2.57357144824417E-20));
#5070=DIRECTION('',(0.999999998147046,6.0876171481578E-5,4.44089209027163E-16));
#5071=DIRECTION('',(-6.0876171481578E-5,0.999999998147046,-2.57357144824417E-20));
#5072=DIRECTION('',(0.999999998147046,6.0876171481578E-5,4.44089209027163E-16));
#5073=DIRECTION('',(-6.0876171481578E-5,0.999999998147046,-2.57357144824417E-20));
#5074=DIRECTION('',(0.999999998147046,6.0876171481578E-5,4.44089209027163E-16));
#5075=DIRECTION('',(-4.44076849609288E-16,-2.03039029105186E-16,1.));
#5076=DIRECTION('',(0.999999998147046,6.08761714816131E-5,4.44089209025187E-16));
#5077=DIRECTION('',(-4.44094428050692E-16,8.571831301492E-17,1.));
#5078=DIRECTION('',(0.999999998147046,6.08761714815767E-5,4.44089209025083E-16));
#5079=DIRECTION('',(-4.44185120529697E-16,-4.60171356356867E-15,1.));
#5080=DIRECTION('',(0.999999998147046,6.0876171481578E-5,4.44465254410647E-16));
#5081=DIRECTION('',(-4.44087286008842E-16,-3.16024907168712E-17,1.));
#5082=DIRECTION('',(0.999999998147046,6.08761714816128E-5,4.44089209024613E-16));
#5083=DIRECTION('',(1.93280829838024E-16,9.27303962655153E-23,0.999999999999994));
#5084=DIRECTION('',(1.,-8.60409291557348E-16,-1.80411241501587E-16));
#5085=DIRECTION('',(-0.999999998147046,-6.08761714818277E-5,-4.44089209200552E-16));
#5086=DIRECTION('',(-4.44083995040506E-16,-8.56654218933077E-17,1.));
#5087=DIRECTION('',(-6.08761714816129E-5,0.999999998147046,1.17266642485094E-16));
#5088=DIRECTION('',(0.999999998147046,6.08761714816129E-5,4.44448351819699E-16));
#5089=DIRECTION('',(6.08761714816144E-5,-0.999999998147046,-1.17293765838873E-16));
#5090=DIRECTION('',(0.999999998147046,6.08761714816144E-5,4.44089209027163E-16));
#5091=DIRECTION('',(-0.999999998147046,-6.0876171481578E-5,-4.44089209027159E-16));
#5092=DIRECTION('',(-4.4408399486875E-16,-8.56653950099378E-17,1.));
#5093=DIRECTION('',(-4.44082064587872E-16,-1.17373673775885E-16,1.));
#5094=DIRECTION('',(0.999999998147046,6.0876171481613E-5,4.440892090249E-16));
#5095=DIRECTION('',(-4.44082067814151E-16,-1.17320713545825E-16,1.));
#5096=DIRECTION('',(0.999999998147046,6.08761714816144E-5,4.44089209027163E-16));
#5097=DIRECTION('',(-4.44426823605847E-16,6.897661130246E-23,1.));
#5098=DIRECTION('',(0.999999998147046,6.08761714815766E-5,4.44426822778145E-16));
#5099=DIRECTION('',(-4.44083995047419E-16,-8.5665308427967E-17,1.));
#5100=DIRECTION('',(0.999999998147046,6.08761714818278E-5,4.44089209200558E-16));
#5101=DIRECTION('',(-4.44083994873641E-16,-8.56653147352083E-17,1.));
#5102=DIRECTION('',(0.999999998147046,6.0876171481578E-5,4.44089209027163E-16));
#5103=DIRECTION('',(6.08761714815766E-5,-0.999999998147046,5.40668696684198E-20));
#5104=DIRECTION('',(0.999999998147046,6.08761714815766E-5,4.43730067880427E-16));
#5105=DIRECTION('',(-6.0876171481578E-5,0.999999998147046,-2.69914374984392E-20));
#5106=DIRECTION('',(0.999999998147046,6.0876171481578E-5,4.44089209027163E-16));
#5107=DIRECTION('',(-4.44089209776623E-16,-1.20600600426608E-21,1.));
#5108=DIRECTION('',(0.999999998147046,6.0876171481578E-5,4.44089209027163E-16));
#5109=DIRECTION('',(3.82689716088827E-16,9.27303996680919E-23,0.999999999999994));
#5110=DIRECTION('',(0.999999999999999,-1.74857415873033E-15,7.63278329429777E-17));
#5111=DIRECTION('',(6.08761714818902E-5,-0.999999998147039,4.51605635229633E-15));
#5112=DIRECTION('',(0.999999996294091,6.08761713686741E-5,-6.08761714852013E-5));
#5113=DIRECTION('',(1.45727232271176E-16,4.39867462719385E-15,0.999999999999994));
#5114=DIRECTION('',(0.999999999999999,-3.08084178828053E-15,-1.45716771982045E-16));
#5115=DIRECTION('',(1.80264996261335E-16,4.57011116558217E-15,0.999999999999999));
#5116=DIRECTION('',(0.999999999999999,-3.19187086700661E-15,-1.21430643318369E-16));
#5117=DIRECTION('',(3.18130182597684E-16,4.57011116558217E-15,0.999999999999999));
#5118=DIRECTION('',(0.999999999999999,-4.85721218020794E-15,1.56125112837924E-16));
#5119=DIRECTION('',(2.72088372242159E-15,4.68743196931399E-15,0.999999999999998));
#5120=DIRECTION('',(0.999999999999997,-4.85721218020793E-15,7.11236625150501E-16));
#5121=DIRECTION('',(2.58301853608524E-15,4.68743196931399E-15,0.999999999999998));
#5122=DIRECTION('',(0.999999999999997,-3.19187086700661E-15,4.33680868994208E-16));
#5123=DIRECTION('',(6.08761714821402E-5,-0.999999998147042,4.51605635819006E-15));
#5124=DIRECTION('',(0.999999996294088,6.08761713658461E-5,-6.08761714803229E-5));
#5125=DIRECTION('',(3.27907881827669E-15,4.3986746271939E-15,0.999999999999994));
#5126=DIRECTION('',(0.999999999999998,-5.27353903817879E-15,1.59941504485061E-15));
#5127=DIRECTION('',(6.08761714800101E-5,-0.999999998147041,4.40963463504513E-15));
#5128=DIRECTION('',(0.999495958104873,6.08454874478476E-5,0.0317462758421725));
#5129=DIRECTION('',(6.08761714821402E-5,-0.999999998147041,4.51605635819006E-15));
#5130=DIRECTION('',(0.999999996294088,6.08761713658461E-5,-6.08761714803229E-5));
#5131=CARTESIAN_POINT('',(0.,0.,0.));
#5132=CARTESIAN_POINT('',(0.,0.,0.));
#5133=CARTESIAN_POINT('Origin',(0.06855,-0.1092,0.02565));
#5134=CARTESIAN_POINT('',(0.06855,-0.0842,0.043125));
#5135=CARTESIAN_POINT('',(0.06855,-0.0842,0.008175));
#5136=CARTESIAN_POINT('',(0.06855,-0.0842,0.02565));
#5137=CARTESIAN_POINT('',(0.06855,-0.1092,0.043125));
#5138=CARTESIAN_POINT('',(0.06855,-0.1092,0.043125));
#5139=CARTESIAN_POINT('',(0.06855,-0.1092,0.008175));
#5140=CARTESIAN_POINT('',(0.06855,-0.1092,0.02565));
#5141=CARTESIAN_POINT('',(0.06855,-0.1092,0.008175));
#5142=CARTESIAN_POINT('Origin',(0.05755,-0.1092,-0.014825));
#5143=CARTESIAN_POINT('',(0.03855,-0.1092,-0.014825));
#5144=CARTESIAN_POINT('',(0.02155,-0.1092,-0.014825));
#5145=CARTESIAN_POINT('',(0.05755,-0.1092,-0.014825));
#5146=CARTESIAN_POINT('',(0.02155,-0.0842,-0.014825));
#5147=CARTESIAN_POINT('',(0.02155,-0.1092,-0.014825));
#5148=CARTESIAN_POINT('',(0.03855,-0.0842,-0.014825));
#5149=CARTESIAN_POINT('',(0.05755,-0.0842,-0.014825));
#5150=CARTESIAN_POINT('',(0.03855,-0.0907,-0.014825));
#5151=CARTESIAN_POINT('',(0.03855,-0.1092,-0.014825));
#5152=CARTESIAN_POINT('',(0.03405,-0.0892,-0.014825));
#5153=CARTESIAN_POINT('Origin',(0.03405,-0.0967,-0.014825));
#5154=CARTESIAN_POINT('',(0.03855,-0.1027,-0.014825));
#5155=CARTESIAN_POINT('Origin',(0.03405,-0.0967,-0.014825));
#5156=CARTESIAN_POINT('',(0.03855,-0.1092,-0.014825));
#5157=CARTESIAN_POINT('Origin',(0.05755,-0.1092,0.066125));
#5158=CARTESIAN_POINT('',(0.03855,-0.0842,0.066125));
#5159=CARTESIAN_POINT('',(0.02155,-0.0842,0.066125));
#5160=CARTESIAN_POINT('',(0.05755,-0.0842,0.066125));
#5161=CARTESIAN_POINT('',(0.02155,-0.1092,0.066125));
#5162=CARTESIAN_POINT('',(0.02155,-0.1092,0.066125));
#5163=CARTESIAN_POINT('',(0.03855,-0.1092,0.066125));
#5164=CARTESIAN_POINT('',(0.05755,-0.1092,0.066125));
#5165=CARTESIAN_POINT('',(0.03855,-0.1027,0.066125));
#5166=CARTESIAN_POINT('',(0.03855,-0.1092,0.066125));
#5167=CARTESIAN_POINT('',(0.03405,-0.0892,0.066125));
#5168=CARTESIAN_POINT('Origin',(0.03405,-0.0967,0.066125));
#5169=CARTESIAN_POINT('',(0.03855,-0.0907,0.066125));
#5170=CARTESIAN_POINT('Origin',(0.03405,-0.0967,0.066125));
#5171=CARTESIAN_POINT('',(0.03855,-0.1092,0.066125));
#5172=CARTESIAN_POINT('Origin',(0.05755,-0.1092,0.02565));
#5173=CARTESIAN_POINT('',(0.06355,-0.1092,0.048125));
#5174=CARTESIAN_POINT('Origin',(0.06355,-0.1092,0.043125));
#5175=CARTESIAN_POINT('',(0.04855,-0.1092,0.048125));
#5176=CARTESIAN_POINT('',(0.05605,-0.1092,0.048125));
#5177=CARTESIAN_POINT('',(0.04355,-0.1092,0.053125));
#5178=CARTESIAN_POINT('Origin',(0.04855,-0.1092,0.053125));
#5179=CARTESIAN_POINT('',(0.04355,-0.1092,0.061125));
#5180=CARTESIAN_POINT('',(0.04355,-0.1092,0.057125));
#5181=CARTESIAN_POINT('Origin',(0.03855,-0.1092,0.061125));
#5182=CARTESIAN_POINT('',(0.02155,-0.1092,0.02565));
#5183=CARTESIAN_POINT('',(0.04355,-0.1092,-0.009825));
#5184=CARTESIAN_POINT('Origin',(0.03855,-0.1092,-0.009825));
#5185=CARTESIAN_POINT('',(0.04355,-0.1092,-0.001825));
#5186=CARTESIAN_POINT('',(0.04355,-0.1092,-0.005825));
#5187=CARTESIAN_POINT('',(0.04855,-0.1092,0.003175));
#5188=CARTESIAN_POINT('Origin',(0.04855,-0.1092,-0.001825));
#5189=CARTESIAN_POINT('',(0.06355,-0.1092,0.003175));
#5190=CARTESIAN_POINT('',(0.05605,-0.1092,0.003175));
#5191=CARTESIAN_POINT('Origin',(0.06355,-0.1092,0.008175));
#5192=CARTESIAN_POINT('',(0.05755,-0.1092,0.0329));
#5193=CARTESIAN_POINT('Origin',(0.05755,-0.1092,0.037125));
#5194=CARTESIAN_POINT('',(0.05755,-0.1092,0.00995));
#5195=CARTESIAN_POINT('Origin',(0.05755,-0.1092,0.014175));
#5196=CARTESIAN_POINT('Origin',(0.05755,-0.0842,0.02565));
#5197=CARTESIAN_POINT('',(0.06355,-0.0842,0.003175));
#5198=CARTESIAN_POINT('',(0.04855,-0.0842,0.003175));
#5199=CARTESIAN_POINT('',(0.05605,-0.0842,0.003175));
#5200=CARTESIAN_POINT('',(0.04355,-0.0842,-0.001825));
#5201=CARTESIAN_POINT('Origin',(0.04855,-0.0842,-0.001825));
#5202=CARTESIAN_POINT('',(0.04355,-0.0842,-0.009825));
#5203=CARTESIAN_POINT('',(0.04355,-0.0842,-0.005825));
#5204=CARTESIAN_POINT('Origin',(0.03855,-0.0842,-0.009825));
#5205=CARTESIAN_POINT('',(0.02155,-0.0842,0.02565));
#5206=CARTESIAN_POINT('',(0.04355,-0.0842,0.061125));
#5207=CARTESIAN_POINT('Origin',(0.03855,-0.0842,0.061125));
#5208=CARTESIAN_POINT('',(0.04355,-0.0842,0.053125));
#5209=CARTESIAN_POINT('',(0.04355,-0.0842,0.057125));
#5210=CARTESIAN_POINT('',(0.04855,-0.0842,0.048125));
#5211=CARTESIAN_POINT('Origin',(0.04855,-0.0842,0.053125));
#5212=CARTESIAN_POINT('',(0.06355,-0.0842,0.048125));
#5213=CARTESIAN_POINT('',(0.05605,-0.0842,0.048125));
#5214=CARTESIAN_POINT('Origin',(0.06355,-0.0842,0.043125));
#5215=CARTESIAN_POINT('Origin',(0.06355,-0.0842,0.008175));
#5216=CARTESIAN_POINT('',(0.05755,-0.0842,0.0329));
#5217=CARTESIAN_POINT('Origin',(0.05755,-0.0842,0.037125));
#5218=CARTESIAN_POINT('',(0.05755,-0.0842,0.00995));
#5219=CARTESIAN_POINT('Origin',(0.05755,-0.0842,0.014175));
#5220=CARTESIAN_POINT('Origin',(0.05755,-0.1092,0.037125));
#5221=CARTESIAN_POINT('',(0.05755,-0.1092,0.0329));
#5222=CARTESIAN_POINT('Origin',(0.05755,-0.1092,0.014175));
#5223=CARTESIAN_POINT('',(0.05755,-0.1092,0.00995));
#5224=CARTESIAN_POINT('Origin',(0.02155,-0.1092,0.02565));
#5225=CARTESIAN_POINT('Origin',(0.03405,-0.0967,-0.023875));
#5226=CARTESIAN_POINT('',(0.03405,-0.0892,-0.023875));
#5227=CARTESIAN_POINT('Ctrl Pts',(0.03855,-0.0907,0.066125));
#5228=CARTESIAN_POINT('Ctrl Pts',(0.0387729524989471,-0.0908672143742104,
0.066125));
#5229=CARTESIAN_POINT('Ctrl Pts',(0.0389827504953742,-0.0910443676288105,
0.0661099450879691));
#5230=CARTESIAN_POINT('Ctrl Pts',(0.0399051826894431,-0.0919072239369945,
0.0659940175331532));
#5231=CARTESIAN_POINT('Ctrl Pts',(0.0405168708018142,-0.0927639295079321,
0.0657455865368071));
#5232=CARTESIAN_POINT('Ctrl Pts',(0.0411335425015076,-0.0941822279651364,
0.0654121811456859));
#5233=CARTESIAN_POINT('Ctrl Pts',(0.0412904479475092,-0.0946775248634452,
0.0653090151899698));
#5234=CARTESIAN_POINT('Ctrl Pts',(0.0414987473161672,-0.0956847881043564,
0.065164916792468));
#5235=CARTESIAN_POINT('Ctrl Pts',(0.04155,-0.0961969286843649,0.065125));
#5236=CARTESIAN_POINT('Ctrl Pts',(0.04155,-0.0972030713156352,0.065125));
#5237=CARTESIAN_POINT('Ctrl Pts',(0.0414987473161672,-0.0977152118956436,
0.065164916792468));
#5238=CARTESIAN_POINT('Ctrl Pts',(0.0412904479475092,-0.0987224751365548,
0.0653090151899698));
#5239=CARTESIAN_POINT('Ctrl Pts',(0.0411335425015076,-0.0992177720348636,
0.0654121811456859));
#5240=CARTESIAN_POINT('Ctrl Pts',(0.0405168708018142,-0.100636070492068,
0.0657455865368071));
#5241=CARTESIAN_POINT('Ctrl Pts',(0.039905182689443,-0.101492776063005,
0.0659940175331532));
#5242=CARTESIAN_POINT('Ctrl Pts',(0.0389827504953742,-0.102355632371189,
0.0661099450879691));
#5243=CARTESIAN_POINT('Ctrl Pts',(0.0387729524989471,-0.10253278562579,
0.066125));
#5244=CARTESIAN_POINT('Ctrl Pts',(0.03855,-0.1027,0.066125));
#5245=CARTESIAN_POINT('Ctrl Pts',(0.03855,-0.1027,-0.014825));
#5246=CARTESIAN_POINT('Ctrl Pts',(0.0387729524989471,-0.10253278562579,
-0.014825));
#5247=CARTESIAN_POINT('Ctrl Pts',(0.0389827504953742,-0.102355632371189,
-0.0148099450879691));
#5248=CARTESIAN_POINT('Ctrl Pts',(0.0399051826894431,-0.101492776063005,
-0.0146940175331532));
#5249=CARTESIAN_POINT('Ctrl Pts',(0.0405168708018142,-0.100636070492068,
-0.0144455865368071));
#5250=CARTESIAN_POINT('Ctrl Pts',(0.0411335425015076,-0.0992177720348636,
-0.0141121811456859));
#5251=CARTESIAN_POINT('Ctrl Pts',(0.0412904479475092,-0.0987224751365548,
-0.0140090151899698));
#5252=CARTESIAN_POINT('Ctrl Pts',(0.0414987473161672,-0.0977152118956436,
-0.013864916792468));
#5253=CARTESIAN_POINT('Ctrl Pts',(0.04155,-0.0972030713156352,-0.013825));
#5254=CARTESIAN_POINT('Ctrl Pts',(0.04155,-0.0961969286843649,-0.013825));
#5255=CARTESIAN_POINT('Ctrl Pts',(0.0414987473161672,-0.0956847881043564,
-0.013864916792468));
#5256=CARTESIAN_POINT('Ctrl Pts',(0.0412904479475093,-0.0946775248634452,
-0.0140090151899698));
#5257=CARTESIAN_POINT('Ctrl Pts',(0.0411335425015076,-0.0941822279651364,
-0.0141121811456859));
#5258=CARTESIAN_POINT('Ctrl Pts',(0.0405168708018142,-0.0927639295079321,
-0.0144455865368071));
#5259=CARTESIAN_POINT('Ctrl Pts',(0.0399051826894431,-0.0919072239369945,
-0.0146940175331532));
#5260=CARTESIAN_POINT('Ctrl Pts',(0.0389827504953742,-0.0910443676288105,
-0.0148099450879691));
#5261=CARTESIAN_POINT('Ctrl Pts',(0.0387729524989471,-0.0908672143742103,
-0.014825));
#5262=CARTESIAN_POINT('Ctrl Pts',(0.03855,-0.0907,-0.014825));
#5263=CARTESIAN_POINT('Origin',(0.05605,-0.0842,0.003175));
#5264=CARTESIAN_POINT('',(0.04855,-0.0842,0.003175));
#5265=CARTESIAN_POINT('',(0.06355,-0.0842,0.003175));
#5266=CARTESIAN_POINT('Origin',(0.04355,-0.0842,-0.005825));
#5267=CARTESIAN_POINT('',(0.04355,-0.0842,-0.001825));
#5268=CARTESIAN_POINT('',(0.04355,-0.0842,-0.009825));
#5269=CARTESIAN_POINT('Origin',(0.05605,-0.0842,0.048125));
#5270=CARTESIAN_POINT('',(0.06355,-0.0842,0.048125));
#5271=CARTESIAN_POINT('',(0.04855,-0.0842,0.048125));
#5272=CARTESIAN_POINT('Origin',(0.04355,-0.0842,0.057125));
#5273=CARTESIAN_POINT('',(0.04355,-0.0842,0.053125));
#5274=CARTESIAN_POINT('',(0.04355,-0.0842,0.061125));
#5275=CARTESIAN_POINT('Origin',(0.06355,-0.1092,0.008175));
#5276=CARTESIAN_POINT('Origin',(0.03855,-0.0842,-0.009825));
#5277=CARTESIAN_POINT('Origin',(0.04855,-0.0842,-0.001825));
#5278=CARTESIAN_POINT('Origin',(0.03855,-0.1092,0.061125));
#5279=CARTESIAN_POINT('Origin',(0.04855,-0.0842,0.053125));
#5280=CARTESIAN_POINT('Origin',(0.06355,-0.0842,0.043125));
#5281=CARTESIAN_POINT('',(0.,0.,0.));
#5282=CARTESIAN_POINT('Origin',(-0.06855,0.1092,0.02565));
#5283=CARTESIAN_POINT('',(-0.06855,0.0842,0.043125));
#5284=CARTESIAN_POINT('',(-0.06855,0.0842,0.008175));
#5285=CARTESIAN_POINT('',(-0.06855,0.0842,0.02565));
#5286=CARTESIAN_POINT('',(-0.06855,0.1092,0.043125));
#5287=CARTESIAN_POINT('',(-0.06855,0.1092,0.043125));
#5288=CARTESIAN_POINT('',(-0.06855,0.1092,0.008175));
#5289=CARTESIAN_POINT('',(-0.06855,0.1092,0.02565));
#5290=CARTESIAN_POINT('',(-0.06855,0.1092,0.008175));
#5291=CARTESIAN_POINT('Origin',(-0.05755,0.1092,-0.014825));
#5292=CARTESIAN_POINT('',(-0.03855,0.1092,-0.014825));
#5293=CARTESIAN_POINT('',(-0.02155,0.1092,-0.014825));
#5294=CARTESIAN_POINT('',(-0.05755,0.1092,-0.014825));
#5295=CARTESIAN_POINT('',(-0.02155,0.0842,-0.014825));
#5296=CARTESIAN_POINT('',(-0.02155,0.1092,-0.014825));
#5297=CARTESIAN_POINT('',(-0.03855,0.0842,-0.014825));
#5298=CARTESIAN_POINT('',(-0.05755,0.0842,-0.014825));
#5299=CARTESIAN_POINT('',(-0.03855,0.0907,-0.014825));
#5300=CARTESIAN_POINT('',(-0.03855,0.1092,-0.014825));
#5301=CARTESIAN_POINT('',(-0.03405,0.0892,-0.014825));
#5302=CARTESIAN_POINT('Origin',(-0.03405,0.0967,-0.014825));
#5303=CARTESIAN_POINT('',(-0.03855,0.1027,-0.014825));
#5304=CARTESIAN_POINT('Origin',(-0.03405,0.0967,-0.014825));
#5305=CARTESIAN_POINT('',(-0.03855,0.1092,-0.014825));
#5306=CARTESIAN_POINT('Origin',(-0.05755,0.1092,0.066125));
#5307=CARTESIAN_POINT('',(-0.03855,0.0842,0.066125));
#5308=CARTESIAN_POINT('',(-0.02155,0.0842,0.066125));
#5309=CARTESIAN_POINT('',(-0.05755,0.0842,0.066125));
#5310=CARTESIAN_POINT('',(-0.02155,0.1092,0.066125));
#5311=CARTESIAN_POINT('',(-0.02155,0.1092,0.066125));
#5312=CARTESIAN_POINT('',(-0.03855,0.1092,0.066125));
#5313=CARTESIAN_POINT('',(-0.05755,0.1092,0.066125));
#5314=CARTESIAN_POINT('',(-0.03855,0.1027,0.066125));
#5315=CARTESIAN_POINT('',(-0.03855,0.1092,0.066125));
#5316=CARTESIAN_POINT('',(-0.03405,0.0892,0.066125));
#5317=CARTESIAN_POINT('Origin',(-0.03405,0.0967,0.066125));
#5318=CARTESIAN_POINT('',(-0.03855,0.0907,0.066125));
#5319=CARTESIAN_POINT('Origin',(-0.03405,0.0967,0.066125));
#5320=CARTESIAN_POINT('',(-0.03855,0.1092,0.066125));
#5321=CARTESIAN_POINT('Origin',(-0.05755,0.1092,0.02565));
#5322=CARTESIAN_POINT('',(-0.06355,0.1092,0.048125));
#5323=CARTESIAN_POINT('Origin',(-0.06355,0.1092,0.043125));
#5324=CARTESIAN_POINT('',(-0.04855,0.1092,0.048125));
#5325=CARTESIAN_POINT('',(-0.05605,0.1092,0.048125));
#5326=CARTESIAN_POINT('',(-0.04355,0.1092,0.053125));
#5327=CARTESIAN_POINT('Origin',(-0.04855,0.1092,0.053125));
#5328=CARTESIAN_POINT('',(-0.04355,0.1092,0.061125));
#5329=CARTESIAN_POINT('',(-0.04355,0.1092,0.057125));
#5330=CARTESIAN_POINT('Origin',(-0.03855,0.1092,0.061125));
#5331=CARTESIAN_POINT('',(-0.02155,0.1092,0.02565));
#5332=CARTESIAN_POINT('',(-0.04355,0.1092,-0.009825));
#5333=CARTESIAN_POINT('Origin',(-0.03855,0.1092,-0.009825));
#5334=CARTESIAN_POINT('',(-0.04355,0.1092,-0.001825));
#5335=CARTESIAN_POINT('',(-0.04355,0.1092,-0.005825));
#5336=CARTESIAN_POINT('',(-0.04855,0.1092,0.003175));
#5337=CARTESIAN_POINT('Origin',(-0.04855,0.1092,-0.001825));
#5338=CARTESIAN_POINT('',(-0.06355,0.1092,0.003175));
#5339=CARTESIAN_POINT('',(-0.05605,0.1092,0.003175));
#5340=CARTESIAN_POINT('Origin',(-0.06355,0.1092,0.008175));
#5341=CARTESIAN_POINT('',(-0.05755,0.1092,0.0329));
#5342=CARTESIAN_POINT('Origin',(-0.05755,0.1092,0.037125));
#5343=CARTESIAN_POINT('',(-0.05755,0.1092,0.00995));
#5344=CARTESIAN_POINT('Origin',(-0.05755,0.1092,0.014175));
#5345=CARTESIAN_POINT('Origin',(-0.05755,0.0842,0.02565));
#5346=CARTESIAN_POINT('',(-0.06355,0.0842,0.003175));
#5347=CARTESIAN_POINT('',(-0.04855,0.0842,0.003175));
#5348=CARTESIAN_POINT('',(-0.05605,0.0842,0.003175));
#5349=CARTESIAN_POINT('',(-0.04355,0.0842,-0.001825));
#5350=CARTESIAN_POINT('Origin',(-0.04855,0.0842,-0.001825));
#5351=CARTESIAN_POINT('',(-0.04355,0.0842,-0.009825));
#5352=CARTESIAN_POINT('',(-0.04355,0.0842,-0.005825));
#5353=CARTESIAN_POINT('Origin',(-0.03855,0.0842,-0.009825));
#5354=CARTESIAN_POINT('',(-0.02155,0.0842,0.02565));
#5355=CARTESIAN_POINT('',(-0.04355,0.0842,0.061125));
#5356=CARTESIAN_POINT('Origin',(-0.03855,0.0842,0.061125));
#5357=CARTESIAN_POINT('',(-0.04355,0.0842,0.053125));
#5358=CARTESIAN_POINT('',(-0.04355,0.0842,0.057125));
#5359=CARTESIAN_POINT('',(-0.04855,0.0842,0.048125));
#5360=CARTESIAN_POINT('Origin',(-0.04855,0.0842,0.053125));
#5361=CARTESIAN_POINT('',(-0.06355,0.0842,0.048125));
#5362=CARTESIAN_POINT('',(-0.05605,0.0842,0.048125));
#5363=CARTESIAN_POINT('Origin',(-0.06355,0.0842,0.043125));
#5364=CARTESIAN_POINT('Origin',(-0.06355,0.0842,0.008175));
#5365=CARTESIAN_POINT('',(-0.05755,0.0842,0.0329));
#5366=CARTESIAN_POINT('Origin',(-0.05755,0.0842,0.037125));
#5367=CARTESIAN_POINT('',(-0.05755,0.0842,0.00995));
#5368=CARTESIAN_POINT('Origin',(-0.05755,0.0842,0.014175));
#5369=CARTESIAN_POINT('Origin',(-0.05755,0.1092,0.037125));
#5370=CARTESIAN_POINT('',(-0.05755,0.1092,0.0329));
#5371=CARTESIAN_POINT('Origin',(-0.05755,0.1092,0.014175));
#5372=CARTESIAN_POINT('',(-0.05755,0.1092,0.00995));
#5373=CARTESIAN_POINT('Origin',(-0.02155,0.1092,0.02565));
#5374=CARTESIAN_POINT('Origin',(-0.03405,0.0967,-0.023875));
#5375=CARTESIAN_POINT('',(-0.03405,0.0892,-0.023875));
#5376=CARTESIAN_POINT('Ctrl Pts',(-0.03855,0.0907,0.066125));
#5377=CARTESIAN_POINT('Ctrl Pts',(-0.0387729524989471,0.0908672143742104,
0.066125));
#5378=CARTESIAN_POINT('Ctrl Pts',(-0.0389827504953742,0.0910443676288105,
0.0661099450879691));
#5379=CARTESIAN_POINT('Ctrl Pts',(-0.0399051826894431,0.0919072239369945,
0.0659940175331532));
#5380=CARTESIAN_POINT('Ctrl Pts',(-0.0405168708018142,0.0927639295079321,
0.0657455865368071));
#5381=CARTESIAN_POINT('Ctrl Pts',(-0.0411335425015076,0.0941822279651364,
0.0654121811456859));
#5382=CARTESIAN_POINT('Ctrl Pts',(-0.0412904479475092,0.0946775248634452,
0.0653090151899698));
#5383=CARTESIAN_POINT('Ctrl Pts',(-0.0414987473161672,0.0956847881043564,
0.065164916792468));
#5384=CARTESIAN_POINT('Ctrl Pts',(-0.04155,0.0961969286843649,0.065125));
#5385=CARTESIAN_POINT('Ctrl Pts',(-0.04155,0.0972030713156352,0.065125));
#5386=CARTESIAN_POINT('Ctrl Pts',(-0.0414987473161672,0.0977152118956436,
0.065164916792468));
#5387=CARTESIAN_POINT('Ctrl Pts',(-0.0412904479475092,0.0987224751365548,
0.0653090151899698));
#5388=CARTESIAN_POINT('Ctrl Pts',(-0.0411335425015076,0.0992177720348636,
0.0654121811456859));
#5389=CARTESIAN_POINT('Ctrl Pts',(-0.0405168708018142,0.100636070492068,
0.0657455865368071));
#5390=CARTESIAN_POINT('Ctrl Pts',(-0.039905182689443,0.101492776063005,
0.0659940175331532));
#5391=CARTESIAN_POINT('Ctrl Pts',(-0.0389827504953742,0.102355632371189,
0.0661099450879691));
#5392=CARTESIAN_POINT('Ctrl Pts',(-0.0387729524989471,0.10253278562579,
0.066125));
#5393=CARTESIAN_POINT('Ctrl Pts',(-0.03855,0.1027,0.066125));
#5394=CARTESIAN_POINT('Ctrl Pts',(-0.03855,0.1027,-0.014825));
#5395=CARTESIAN_POINT('Ctrl Pts',(-0.0387729524989471,0.10253278562579,
-0.014825));
#5396=CARTESIAN_POINT('Ctrl Pts',(-0.0389827504953742,0.102355632371189,
-0.0148099450879691));
#5397=CARTESIAN_POINT('Ctrl Pts',(-0.0399051826894431,0.101492776063005,
-0.0146940175331532));
#5398=CARTESIAN_POINT('Ctrl Pts',(-0.0405168708018142,0.100636070492068,
-0.0144455865368071));
#5399=CARTESIAN_POINT('Ctrl Pts',(-0.0411335425015076,0.0992177720348636,
-0.0141121811456859));
#5400=CARTESIAN_POINT('Ctrl Pts',(-0.0412904479475092,0.0987224751365548,
-0.0140090151899698));
#5401=CARTESIAN_POINT('Ctrl Pts',(-0.0414987473161672,0.0977152118956436,
-0.013864916792468));
#5402=CARTESIAN_POINT('Ctrl Pts',(-0.04155,0.0972030713156352,-0.013825));
#5403=CARTESIAN_POINT('Ctrl Pts',(-0.04155,0.0961969286843649,-0.013825));
#5404=CARTESIAN_POINT('Ctrl Pts',(-0.0414987473161672,0.0956847881043564,
-0.013864916792468));
#5405=CARTESIAN_POINT('Ctrl Pts',(-0.0412904479475093,0.0946775248634452,
-0.0140090151899698));
#5406=CARTESIAN_POINT('Ctrl Pts',(-0.0411335425015076,0.0941822279651364,
-0.0141121811456859));
#5407=CARTESIAN_POINT('Ctrl Pts',(-0.0405168708018142,0.0927639295079321,
-0.0144455865368071));
#5408=CARTESIAN_POINT('Ctrl Pts',(-0.0399051826894431,0.0919072239369945,
-0.0146940175331532));
#5409=CARTESIAN_POINT('Ctrl Pts',(-0.0389827504953742,0.0910443676288105,
-0.0148099450879691));
#5410=CARTESIAN_POINT('Ctrl Pts',(-0.0387729524989471,0.0908672143742103,
-0.014825));
#5411=CARTESIAN_POINT('Ctrl Pts',(-0.03855,0.0907,-0.014825));
#5412=CARTESIAN_POINT('Origin',(-0.05605,0.0842,0.003175));
#5413=CARTESIAN_POINT('',(-0.04855,0.0842,0.003175));
#5414=CARTESIAN_POINT('',(-0.06355,0.0842,0.003175));
#5415=CARTESIAN_POINT('Origin',(-0.04355,0.0842,-0.005825));
#5416=CARTESIAN_POINT('',(-0.04355,0.0842,-0.001825));
#5417=CARTESIAN_POINT('',(-0.04355,0.0842,-0.009825));
#5418=CARTESIAN_POINT('Origin',(-0.05605,0.0842,0.048125));
#5419=CARTESIAN_POINT('',(-0.06355,0.0842,0.048125));
#5420=CARTESIAN_POINT('',(-0.04855,0.0842,0.048125));
#5421=CARTESIAN_POINT('Origin',(-0.04355,0.0842,0.057125));
#5422=CARTESIAN_POINT('',(-0.04355,0.0842,0.053125));
#5423=CARTESIAN_POINT('',(-0.04355,0.0842,0.061125));
#5424=CARTESIAN_POINT('Origin',(-0.06355,0.1092,0.008175));
#5425=CARTESIAN_POINT('Origin',(-0.03855,0.0842,-0.009825));
#5426=CARTESIAN_POINT('Origin',(-0.04855,0.0842,-0.001825));
#5427=CARTESIAN_POINT('Origin',(-0.03855,0.1092,0.061125));
#5428=CARTESIAN_POINT('Origin',(-0.04855,0.0842,0.053125));
#5429=CARTESIAN_POINT('Origin',(-0.06355,0.0842,0.043125));
#5430=CARTESIAN_POINT('',(0.,0.,0.));
#5431=CARTESIAN_POINT('Origin',(-0.06855,-0.1092,0.02565));
#5432=CARTESIAN_POINT('',(-0.06855,-0.0842,0.043125));
#5433=CARTESIAN_POINT('',(-0.06855,-0.0842,0.008175));
#5434=CARTESIAN_POINT('',(-0.06855,-0.0842,0.02565));
#5435=CARTESIAN_POINT('',(-0.06855,-0.1092,0.008175));
#5436=CARTESIAN_POINT('',(-0.06855,-0.1092,0.008175));
#5437=CARTESIAN_POINT('',(-0.06855,-0.1092,0.043125));
#5438=CARTESIAN_POINT('',(-0.06855,-0.1092,0.02565));
#5439=CARTESIAN_POINT('',(-0.06855,-0.1092,0.043125));
#5440=CARTESIAN_POINT('Origin',(-0.05755,-0.1092,-0.014825));
#5441=CARTESIAN_POINT('',(-0.03855,-0.1092,-0.014825));
#5442=CARTESIAN_POINT('',(-0.02155,-0.1092,-0.014825));
#5443=CARTESIAN_POINT('',(-0.05755,-0.1092,-0.014825));
#5444=CARTESIAN_POINT('',(-0.03855,-0.1027,-0.014825));
#5445=CARTESIAN_POINT('',(-0.03855,-0.1092,-0.014825));
#5446=CARTESIAN_POINT('',(-0.03405,-0.0892,-0.014825));
#5447=CARTESIAN_POINT('Origin',(-0.03405,-0.0967,-0.014825));
#5448=CARTESIAN_POINT('',(-0.03855,-0.0907,-0.014825));
#5449=CARTESIAN_POINT('Origin',(-0.03405,-0.0967,-0.014825));
#5450=CARTESIAN_POINT('',(-0.03855,-0.0842,-0.014825));
#5451=CARTESIAN_POINT('',(-0.03855,-0.1092,-0.014825));
#5452=CARTESIAN_POINT('',(-0.02155,-0.0842,-0.014825));
#5453=CARTESIAN_POINT('',(-0.05755,-0.0842,-0.014825));
#5454=CARTESIAN_POINT('',(-0.02155,-0.1092,-0.014825));
#5455=CARTESIAN_POINT('Origin',(-0.05755,-0.1092,0.066125));
#5456=CARTESIAN_POINT('',(-0.03855,-0.0842,0.066125));
#5457=CARTESIAN_POINT('',(-0.02155,-0.0842,0.066125));
#5458=CARTESIAN_POINT('',(-0.05755,-0.0842,0.066125));
#5459=CARTESIAN_POINT('',(-0.03855,-0.0907,0.066125));
#5460=CARTESIAN_POINT('',(-0.03855,-0.1092,0.066125));
#5461=CARTESIAN_POINT('',(-0.03405,-0.0892,0.066125));
#5462=CARTESIAN_POINT('Origin',(-0.03405,-0.0967,0.066125));
#5463=CARTESIAN_POINT('',(-0.03855,-0.1027,0.066125));
#5464=CARTESIAN_POINT('Origin',(-0.03405,-0.0967,0.066125));
#5465=CARTESIAN_POINT('',(-0.03855,-0.1092,0.066125));
#5466=CARTESIAN_POINT('',(-0.03855,-0.1092,0.066125));
#5467=CARTESIAN_POINT('',(-0.02155,-0.1092,0.066125));
#5468=CARTESIAN_POINT('',(-0.05755,-0.1092,0.066125));
#5469=CARTESIAN_POINT('',(-0.02155,-0.1092,0.066125));
#5470=CARTESIAN_POINT('Origin',(-0.05755,-0.1092,0.02565));
#5471=CARTESIAN_POINT('',(-0.06355,-0.1092,0.003175));
#5472=CARTESIAN_POINT('Origin',(-0.06355,-0.1092,0.008175));
#5473=CARTESIAN_POINT('',(-0.04855,-0.1092,0.003175));
#5474=CARTESIAN_POINT('',(-0.05605,-0.1092,0.003175));
#5475=CARTESIAN_POINT('',(-0.04355,-0.1092,-0.001825));
#5476=CARTESIAN_POINT('Origin',(-0.04855,-0.1092,-0.001825));
#5477=CARTESIAN_POINT('',(-0.04355,-0.1092,-0.009825));
#5478=CARTESIAN_POINT('',(-0.04355,-0.1092,-0.005825));
#5479=CARTESIAN_POINT('Origin',(-0.03855,-0.1092,-0.009825));
#5480=CARTESIAN_POINT('',(-0.02155,-0.1092,0.02565));
#5481=CARTESIAN_POINT('',(-0.04355,-0.1092,0.061125));
#5482=CARTESIAN_POINT('Origin',(-0.03855,-0.1092,0.061125));
#5483=CARTESIAN_POINT('',(-0.04355,-0.1092,0.053125));
#5484=CARTESIAN_POINT('',(-0.04355,-0.1092,0.057125));
#5485=CARTESIAN_POINT('',(-0.04855,-0.1092,0.048125));
#5486=CARTESIAN_POINT('Origin',(-0.04855,-0.1092,0.053125));
#5487=CARTESIAN_POINT('',(-0.06355,-0.1092,0.048125));
#5488=CARTESIAN_POINT('',(-0.05605,-0.1092,0.048125));
#5489=CARTESIAN_POINT('Origin',(-0.06355,-0.1092,0.043125));
#5490=CARTESIAN_POINT('',(-0.05755,-0.1092,0.0329));
#5491=CARTESIAN_POINT('Origin',(-0.05755,-0.1092,0.037125));
#5492=CARTESIAN_POINT('',(-0.05755,-0.1092,0.00995));
#5493=CARTESIAN_POINT('Origin',(-0.05755,-0.1092,0.014175));
#5494=CARTESIAN_POINT('Origin',(-0.05755,-0.0842,0.02565));
#5495=CARTESIAN_POINT('',(-0.06355,-0.0842,0.003175));
#5496=CARTESIAN_POINT('',(-0.04855,-0.0842,0.003175));
#5497=CARTESIAN_POINT('',(-0.05605,-0.0842,0.003175));
#5498=CARTESIAN_POINT('Origin',(-0.06355,-0.0842,0.008175));
#5499=CARTESIAN_POINT('',(-0.06355,-0.0842,0.048125));
#5500=CARTESIAN_POINT('Origin',(-0.06355,-0.0842,0.043125));
#5501=CARTESIAN_POINT('',(-0.04855,-0.0842,0.048125));
#5502=CARTESIAN_POINT('',(-0.05605,-0.0842,0.048125));
#5503=CARTESIAN_POINT('',(-0.04355,-0.0842,0.053125));
#5504=CARTESIAN_POINT('Origin',(-0.04855,-0.0842,0.053125));
#5505=CARTESIAN_POINT('',(-0.04355,-0.0842,0.061125));
#5506=CARTESIAN_POINT('',(-0.04355,-0.0842,0.057125));
#5507=CARTESIAN_POINT('Origin',(-0.03855,-0.0842,0.061125));
#5508=CARTESIAN_POINT('',(-0.02155,-0.0842,0.02565));
#5509=CARTESIAN_POINT('',(-0.04355,-0.0842,-0.009825));
#5510=CARTESIAN_POINT('Origin',(-0.03855,-0.0842,-0.009825));
#5511=CARTESIAN_POINT('',(-0.04355,-0.0842,-0.001825));
#5512=CARTESIAN_POINT('',(-0.04355,-0.0842,-0.005825));
#5513=CARTESIAN_POINT('Origin',(-0.04855,-0.0842,-0.001825));
#5514=CARTESIAN_POINT('',(-0.05755,-0.0842,0.0329));
#5515=CARTESIAN_POINT('Origin',(-0.05755,-0.0842,0.037125));
#5516=CARTESIAN_POINT('',(-0.05755,-0.0842,0.00995));
#5517=CARTESIAN_POINT('Origin',(-0.05755,-0.0842,0.014175));
#5518=CARTESIAN_POINT('Origin',(-0.05755,-0.1092,0.037125));
#5519=CARTESIAN_POINT('',(-0.05755,-0.1092,0.0329));
#5520=CARTESIAN_POINT('Origin',(-0.05755,-0.1092,0.014175));
#5521=CARTESIAN_POINT('',(-0.05755,-0.1092,0.00995));
#5522=CARTESIAN_POINT('Origin',(-0.02155,-0.1092,0.02565));
#5523=CARTESIAN_POINT('Origin',(-0.03405,-0.0967,-0.023875));
#5524=CARTESIAN_POINT('Ctrl Pts',(-0.03855,-0.1027,-0.014825));
#5525=CARTESIAN_POINT('Ctrl Pts',(-0.0387729524989471,-0.10253278562579,
-0.014825));
#5526=CARTESIAN_POINT('Ctrl Pts',(-0.0389827504953742,-0.102355632371189,
-0.0148099450879691));
#5527=CARTESIAN_POINT('Ctrl Pts',(-0.0399051826894431,-0.101492776063005,
-0.0146940175331532));
#5528=CARTESIAN_POINT('Ctrl Pts',(-0.0405168708018142,-0.100636070492068,
-0.0144455865368071));
#5529=CARTESIAN_POINT('Ctrl Pts',(-0.0411335425015076,-0.0992177720348636,
-0.0141121811456859));
#5530=CARTESIAN_POINT('Ctrl Pts',(-0.0412904479475092,-0.0987224751365548,
-0.0140090151899698));
#5531=CARTESIAN_POINT('Ctrl Pts',(-0.0414987473161672,-0.0977152118956436,
-0.013864916792468));
#5532=CARTESIAN_POINT('Ctrl Pts',(-0.04155,-0.0972030713156352,-0.013825));
#5533=CARTESIAN_POINT('Ctrl Pts',(-0.04155,-0.0961969286843648,-0.013825));
#5534=CARTESIAN_POINT('Ctrl Pts',(-0.0414987473161672,-0.0956847881043564,
-0.013864916792468));
#5535=CARTESIAN_POINT('Ctrl Pts',(-0.0412904479475093,-0.0946775248634452,
-0.0140090151899698));
#5536=CARTESIAN_POINT('Ctrl Pts',(-0.0411335425015076,-0.0941822279651364,
-0.0141121811456859));
#5537=CARTESIAN_POINT('Ctrl Pts',(-0.0405168708018142,-0.0927639295079321,
-0.0144455865368071));
#5538=CARTESIAN_POINT('Ctrl Pts',(-0.0399051826894431,-0.0919072239369945,
-0.0146940175331532));
#5539=CARTESIAN_POINT('Ctrl Pts',(-0.0389827504953742,-0.0910443676288105,
-0.0148099450879691));
#5540=CARTESIAN_POINT('Ctrl Pts',(-0.0387729524989471,-0.0908672143742103,
-0.014825));
#5541=CARTESIAN_POINT('Ctrl Pts',(-0.03855,-0.0907,-0.014825));
#5542=CARTESIAN_POINT('',(-0.03405,-0.0892,-0.023875));
#5543=CARTESIAN_POINT('Ctrl Pts',(-0.03855,-0.0907,0.066125));
#5544=CARTESIAN_POINT('Ctrl Pts',(-0.0387729524989471,-0.0908672143742103,
0.066125));
#5545=CARTESIAN_POINT('Ctrl Pts',(-0.0389827504953742,-0.0910443676288105,
0.0661099450879691));
#5546=CARTESIAN_POINT('Ctrl Pts',(-0.039905182689443,-0.0919072239369945,
0.0659940175331532));
#5547=CARTESIAN_POINT('Ctrl Pts',(-0.0405168708018142,-0.0927639295079321,
0.0657455865368071));
#5548=CARTESIAN_POINT('Ctrl Pts',(-0.0411335425015076,-0.0941822279651364,
0.0654121811456859));
#5549=CARTESIAN_POINT('Ctrl Pts',(-0.0412904479475093,-0.0946775248634452,
0.0653090151899698));
#5550=CARTESIAN_POINT('Ctrl Pts',(-0.0414987473161672,-0.0956847881043564,
0.065164916792468));
#5551=CARTESIAN_POINT('Ctrl Pts',(-0.04155,-0.0961969286843649,0.065125));
#5552=CARTESIAN_POINT('Ctrl Pts',(-0.04155,-0.0972030713156351,0.065125));
#5553=CARTESIAN_POINT('Ctrl Pts',(-0.0414987473161672,-0.0977152118956436,
0.065164916792468));
#5554=CARTESIAN_POINT('Ctrl Pts',(-0.0412904479475092,-0.0987224751365548,
0.0653090151899699));
#5555=CARTESIAN_POINT('Ctrl Pts',(-0.0411335425015076,-0.0992177720348636,
0.0654121811456859));
#5556=CARTESIAN_POINT('Ctrl Pts',(-0.0405168708018142,-0.100636070492068,
0.0657455865368071));
#5557=CARTESIAN_POINT('Ctrl Pts',(-0.0399051826894431,-0.101492776063005,
0.0659940175331532));
#5558=CARTESIAN_POINT('Ctrl Pts',(-0.0389827504953742,-0.102355632371189,
0.0661099450879691));
#5559=CARTESIAN_POINT('Ctrl Pts',(-0.0387729524989471,-0.10253278562579,
0.066125));
#5560=CARTESIAN_POINT('Ctrl Pts',(-0.03855,-0.1027,0.066125));
#5561=CARTESIAN_POINT('Origin',(-0.05605,-0.0842,0.003175));
#5562=CARTESIAN_POINT('',(-0.06355,-0.0842,0.003175));
#5563=CARTESIAN_POINT('',(-0.04855,-0.0842,0.003175));
#5564=CARTESIAN_POINT('Origin',(-0.04355,-0.0842,-0.005825));
#5565=CARTESIAN_POINT('',(-0.04355,-0.0842,-0.009825));
#5566=CARTESIAN_POINT('',(-0.04355,-0.0842,-0.001825));
#5567=CARTESIAN_POINT('Origin',(-0.05605,-0.0842,0.048125));
#5568=CARTESIAN_POINT('',(-0.04855,-0.0842,0.048125));
#5569=CARTESIAN_POINT('',(-0.06355,-0.0842,0.048125));
#5570=CARTESIAN_POINT('Origin',(-0.04355,-0.0842,0.057125));
#5571=CARTESIAN_POINT('',(-0.04355,-0.0842,0.061125));
#5572=CARTESIAN_POINT('',(-0.04355,-0.0842,0.053125));
#5573=CARTESIAN_POINT('Origin',(-0.06355,-0.1092,0.008175));
#5574=CARTESIAN_POINT('Origin',(-0.03855,-0.0842,-0.009825));
#5575=CARTESIAN_POINT('Origin',(-0.04855,-0.0842,-0.001825));
#5576=CARTESIAN_POINT('Origin',(-0.03855,-0.1092,0.061125));
#5577=CARTESIAN_POINT('Origin',(-0.04855,-0.0842,0.053125));
#5578=CARTESIAN_POINT('Origin',(-0.06355,-0.0842,0.043125));
#5579=CARTESIAN_POINT('',(0.,0.,0.));
#5580=CARTESIAN_POINT('Origin',(0.06855,0.1092,0.02565));
#5581=CARTESIAN_POINT('',(0.06855,0.0842,0.043125));
#5582=CARTESIAN_POINT('',(0.06855,0.0842,0.008175));
#5583=CARTESIAN_POINT('',(0.06855,0.0842,0.02565));
#5584=CARTESIAN_POINT('',(0.06855,0.1092,0.008175));
#5585=CARTESIAN_POINT('',(0.06855,0.1092,0.008175));
#5586=CARTESIAN_POINT('',(0.06855,0.1092,0.043125));
#5587=CARTESIAN_POINT('',(0.06855,0.1092,0.02565));
#5588=CARTESIAN_POINT('',(0.06855,0.1092,0.043125));
#5589=CARTESIAN_POINT('Origin',(0.05755,0.1092,-0.014825));
#5590=CARTESIAN_POINT('',(0.03855,0.1092,-0.014825));
#5591=CARTESIAN_POINT('',(0.02155,0.1092,-0.014825));
#5592=CARTESIAN_POINT('',(0.05755,0.1092,-0.014825));
#5593=CARTESIAN_POINT('',(0.03855,0.1027,-0.014825));
#5594=CARTESIAN_POINT('',(0.03855,0.1092,-0.014825));
#5595=CARTESIAN_POINT('',(0.03405,0.0892,-0.014825));
#5596=CARTESIAN_POINT('Origin',(0.03405,0.0967,-0.014825));
#5597=CARTESIAN_POINT('',(0.03855,0.0907,-0.014825));
#5598=CARTESIAN_POINT('Origin',(0.03405,0.0967,-0.014825));
#5599=CARTESIAN_POINT('',(0.03855,0.0842,-0.014825));
#5600=CARTESIAN_POINT('',(0.03855,0.1092,-0.014825));
#5601=CARTESIAN_POINT('',(0.02155,0.0842,-0.014825));
#5602=CARTESIAN_POINT('',(0.05755,0.0842,-0.014825));
#5603=CARTESIAN_POINT('',(0.02155,0.1092,-0.014825));
#5604=CARTESIAN_POINT('Origin',(0.05755,0.1092,0.066125));
#5605=CARTESIAN_POINT('',(0.03855,0.0842,0.066125));
#5606=CARTESIAN_POINT('',(0.02155,0.0842,0.066125));
#5607=CARTESIAN_POINT('',(0.05755,0.0842,0.066125));
#5608=CARTESIAN_POINT('',(0.03855,0.0907,0.066125));
#5609=CARTESIAN_POINT('',(0.03855,0.1092,0.066125));
#5610=CARTESIAN_POINT('',(0.03405,0.0892,0.066125));
#5611=CARTESIAN_POINT('Origin',(0.03405,0.0967,0.066125));
#5612=CARTESIAN_POINT('',(0.03855,0.1027,0.066125));
#5613=CARTESIAN_POINT('Origin',(0.03405,0.0967,0.066125));
#5614=CARTESIAN_POINT('',(0.03855,0.1092,0.066125));
#5615=CARTESIAN_POINT('',(0.03855,0.1092,0.066125));
#5616=CARTESIAN_POINT('',(0.02155,0.1092,0.066125));
#5617=CARTESIAN_POINT('',(0.05755,0.1092,0.066125));
#5618=CARTESIAN_POINT('',(0.02155,0.1092,0.066125));
#5619=CARTESIAN_POINT('Origin',(0.05755,0.1092,0.02565));
#5620=CARTESIAN_POINT('',(0.06355,0.1092,0.003175));
#5621=CARTESIAN_POINT('Origin',(0.06355,0.1092,0.008175));
#5622=CARTESIAN_POINT('',(0.04855,0.1092,0.003175));
#5623=CARTESIAN_POINT('',(0.05605,0.1092,0.003175));
#5624=CARTESIAN_POINT('',(0.04355,0.1092,-0.001825));
#5625=CARTESIAN_POINT('Origin',(0.04855,0.1092,-0.001825));
#5626=CARTESIAN_POINT('',(0.04355,0.1092,-0.009825));
#5627=CARTESIAN_POINT('',(0.04355,0.1092,-0.005825));
#5628=CARTESIAN_POINT('Origin',(0.03855,0.1092,-0.009825));
#5629=CARTESIAN_POINT('',(0.02155,0.1092,0.02565));
#5630=CARTESIAN_POINT('',(0.04355,0.1092,0.061125));
#5631=CARTESIAN_POINT('Origin',(0.03855,0.1092,0.061125));
#5632=CARTESIAN_POINT('',(0.04355,0.1092,0.053125));
#5633=CARTESIAN_POINT('',(0.04355,0.1092,0.057125));
#5634=CARTESIAN_POINT('',(0.04855,0.1092,0.048125));
#5635=CARTESIAN_POINT('Origin',(0.04855,0.1092,0.053125));
#5636=CARTESIAN_POINT('',(0.06355,0.1092,0.048125));
#5637=CARTESIAN_POINT('',(0.05605,0.1092,0.048125));
#5638=CARTESIAN_POINT('Origin',(0.06355,0.1092,0.043125));
#5639=CARTESIAN_POINT('',(0.05755,0.1092,0.0329));
#5640=CARTESIAN_POINT('Origin',(0.05755,0.1092,0.037125));
#5641=CARTESIAN_POINT('',(0.05755,0.1092,0.00995));
#5642=CARTESIAN_POINT('Origin',(0.05755,0.1092,0.014175));
#5643=CARTESIAN_POINT('Origin',(0.05755,0.0842,0.02565));
#5644=CARTESIAN_POINT('',(0.06355,0.0842,0.003175));
#5645=CARTESIAN_POINT('',(0.04855,0.0842,0.003175));
#5646=CARTESIAN_POINT('',(0.05605,0.0842,0.003175));
#5647=CARTESIAN_POINT('Origin',(0.06355,0.0842,0.008175));
#5648=CARTESIAN_POINT('',(0.06355,0.0842,0.048125));
#5649=CARTESIAN_POINT('Origin',(0.06355,0.0842,0.043125));
#5650=CARTESIAN_POINT('',(0.04855,0.0842,0.048125));
#5651=CARTESIAN_POINT('',(0.05605,0.0842,0.048125));
#5652=CARTESIAN_POINT('',(0.04355,0.0842,0.053125));
#5653=CARTESIAN_POINT('Origin',(0.04855,0.0842,0.053125));
#5654=CARTESIAN_POINT('',(0.04355,0.0842,0.061125));
#5655=CARTESIAN_POINT('',(0.04355,0.0842,0.057125));
#5656=CARTESIAN_POINT('Origin',(0.03855,0.0842,0.061125));
#5657=CARTESIAN_POINT('',(0.02155,0.0842,0.02565));
#5658=CARTESIAN_POINT('',(0.04355,0.0842,-0.009825));
#5659=CARTESIAN_POINT('Origin',(0.03855,0.0842,-0.009825));
#5660=CARTESIAN_POINT('',(0.04355,0.0842,-0.001825));
#5661=CARTESIAN_POINT('',(0.04355,0.0842,-0.005825));
#5662=CARTESIAN_POINT('Origin',(0.04855,0.0842,-0.001825));
#5663=CARTESIAN_POINT('',(0.05755,0.0842,0.0329));
#5664=CARTESIAN_POINT('Origin',(0.05755,0.0842,0.037125));
#5665=CARTESIAN_POINT('',(0.05755,0.0842,0.00995));
#5666=CARTESIAN_POINT('Origin',(0.05755,0.0842,0.014175));
#5667=CARTESIAN_POINT('Origin',(0.05755,0.1092,0.037125));
#5668=CARTESIAN_POINT('',(0.05755,0.1092,0.0329));
#5669=CARTESIAN_POINT('Origin',(0.05755,0.1092,0.014175));
#5670=CARTESIAN_POINT('',(0.05755,0.1092,0.00995));
#5671=CARTESIAN_POINT('Origin',(0.02155,0.1092,0.02565));
#5672=CARTESIAN_POINT('Origin',(0.03405,0.0967,-0.023875));
#5673=CARTESIAN_POINT('Ctrl Pts',(0.03855,0.1027,-0.014825));
#5674=CARTESIAN_POINT('Ctrl Pts',(0.0387729524989471,0.10253278562579,-0.014825));
#5675=CARTESIAN_POINT('Ctrl Pts',(0.0389827504953742,0.102355632371189,
-0.0148099450879691));
#5676=CARTESIAN_POINT('Ctrl Pts',(0.0399051826894431,0.101492776063005,
-0.0146940175331532));
#5677=CARTESIAN_POINT('Ctrl Pts',(0.0405168708018142,0.100636070492068,
-0.0144455865368071));
#5678=CARTESIAN_POINT('Ctrl Pts',(0.0411335425015076,0.0992177720348636,
-0.0141121811456859));
#5679=CARTESIAN_POINT('Ctrl Pts',(0.0412904479475092,0.0987224751365548,
-0.0140090151899698));
#5680=CARTESIAN_POINT('Ctrl Pts',(0.0414987473161672,0.0977152118956436,
-0.013864916792468));
#5681=CARTESIAN_POINT('Ctrl Pts',(0.04155,0.0972030713156352,-0.013825));
#5682=CARTESIAN_POINT('Ctrl Pts',(0.04155,0.0961969286843648,-0.013825));
#5683=CARTESIAN_POINT('Ctrl Pts',(0.0414987473161672,0.0956847881043564,
-0.013864916792468));
#5684=CARTESIAN_POINT('Ctrl Pts',(0.0412904479475093,0.0946775248634452,
-0.0140090151899698));
#5685=CARTESIAN_POINT('Ctrl Pts',(0.0411335425015076,0.0941822279651364,
-0.0141121811456859));
#5686=CARTESIAN_POINT('Ctrl Pts',(0.0405168708018142,0.0927639295079321,
-0.0144455865368071));
#5687=CARTESIAN_POINT('Ctrl Pts',(0.0399051826894431,0.0919072239369945,
-0.0146940175331532));
#5688=CARTESIAN_POINT('Ctrl Pts',(0.0389827504953742,0.0910443676288105,
-0.0148099450879691));
#5689=CARTESIAN_POINT('Ctrl Pts',(0.0387729524989471,0.0908672143742103,
-0.014825));
#5690=CARTESIAN_POINT('Ctrl Pts',(0.03855,0.0907,-0.014825));
#5691=CARTESIAN_POINT('',(0.03405,0.0892,-0.023875));
#5692=CARTESIAN_POINT('Ctrl Pts',(0.03855,0.0907,0.066125));
#5693=CARTESIAN_POINT('Ctrl Pts',(0.0387729524989471,0.0908672143742103,
0.066125));
#5694=CARTESIAN_POINT('Ctrl Pts',(0.0389827504953742,0.0910443676288105,
0.0661099450879691));
#5695=CARTESIAN_POINT('Ctrl Pts',(0.039905182689443,0.0919072239369945,
0.0659940175331532));
#5696=CARTESIAN_POINT('Ctrl Pts',(0.0405168708018142,0.0927639295079321,
0.0657455865368071));
#5697=CARTESIAN_POINT('Ctrl Pts',(0.0411335425015076,0.0941822279651364,
0.0654121811456859));
#5698=CARTESIAN_POINT('Ctrl Pts',(0.0412904479475093,0.0946775248634452,
0.0653090151899698));
#5699=CARTESIAN_POINT('Ctrl Pts',(0.0414987473161672,0.0956847881043564,
0.065164916792468));
#5700=CARTESIAN_POINT('Ctrl Pts',(0.04155,0.0961969286843649,0.065125));
#5701=CARTESIAN_POINT('Ctrl Pts',(0.04155,0.0972030713156351,0.065125));
#5702=CARTESIAN_POINT('Ctrl Pts',(0.0414987473161672,0.0977152118956436,
0.065164916792468));
#5703=CARTESIAN_POINT('Ctrl Pts',(0.0412904479475092,0.0987224751365548,
0.0653090151899699));
#5704=CARTESIAN_POINT('Ctrl Pts',(0.0411335425015076,0.0992177720348636,
0.0654121811456859));
#5705=CARTESIAN_POINT('Ctrl Pts',(0.0405168708018142,0.100636070492068,
0.0657455865368071));
#5706=CARTESIAN_POINT('Ctrl Pts',(0.0399051826894431,0.101492776063005,
0.0659940175331532));
#5707=CARTESIAN_POINT('Ctrl Pts',(0.0389827504953742,0.102355632371189,
0.0661099450879691));
#5708=CARTESIAN_POINT('Ctrl Pts',(0.0387729524989471,0.10253278562579,0.066125));
#5709=CARTESIAN_POINT('Ctrl Pts',(0.03855,0.1027,0.066125));
#5710=CARTESIAN_POINT('Origin',(0.05605,0.0842,0.003175));
#5711=CARTESIAN_POINT('',(0.06355,0.0842,0.003175));
#5712=CARTESIAN_POINT('',(0.04855,0.0842,0.003175));
#5713=CARTESIAN_POINT('Origin',(0.04355,0.0842,-0.005825));
#5714=CARTESIAN_POINT('',(0.04355,0.0842,-0.009825));
#5715=CARTESIAN_POINT('',(0.04355,0.0842,-0.001825));
#5716=CARTESIAN_POINT('Origin',(0.05605,0.0842,0.048125));
#5717=CARTESIAN_POINT('',(0.04855,0.0842,0.048125));
#5718=CARTESIAN_POINT('',(0.06355,0.0842,0.048125));
#5719=CARTESIAN_POINT('Origin',(0.04355,0.0842,0.057125));
#5720=CARTESIAN_POINT('',(0.04355,0.0842,0.061125));
#5721=CARTESIAN_POINT('',(0.04355,0.0842,0.053125));
#5722=CARTESIAN_POINT('Origin',(0.06355,0.1092,0.008175));
#5723=CARTESIAN_POINT('Origin',(0.03855,0.0842,-0.009825));
#5724=CARTESIAN_POINT('Origin',(0.04855,0.0842,-0.001825));
#5725=CARTESIAN_POINT('Origin',(0.03855,0.1092,0.061125));
#5726=CARTESIAN_POINT('Origin',(0.04855,0.0842,0.053125));
#5727=CARTESIAN_POINT('Origin',(0.06355,0.0842,0.043125));
#5728=CARTESIAN_POINT('',(0.,0.,0.));
#5729=CARTESIAN_POINT('',(0.,0.,0.));
#5730=CARTESIAN_POINT('Origin',(0.06655,-0.0172,0.02565));
#5731=CARTESIAN_POINT('',(0.04655,-0.0172,-0.001825));
#5732=CARTESIAN_POINT('',(0.04655,-0.0172,-0.009825));
#5733=CARTESIAN_POINT('',(0.04655,-0.0172,0.02565));
#5734=CARTESIAN_POINT('',(0.06855,-0.0172,-0.009825));
#5735=CARTESIAN_POINT('',(0.04655,-0.0172,-0.009825));
#5736=CARTESIAN_POINT('',(0.06855,-0.0172,-0.001825));
#5737=CARTESIAN_POINT('',(0.06855,-0.0172,0.02565));
#5738=CARTESIAN_POINT('',(0.06655,-0.0172,-0.001825));
#5739=CARTESIAN_POINT('Origin',(0.06655,-0.009975,0.066125));
#5740=CARTESIAN_POINT('',(0.06855,-0.00775,0.066125));
#5741=CARTESIAN_POINT('',(0.06855,-0.0122,0.066125));
#5742=CARTESIAN_POINT('',(0.06855,-0.009975,0.066125));
#5743=CARTESIAN_POINT('',(0.04655,-0.00775,0.066125));
#5744=CARTESIAN_POINT('',(0.06855,-0.00775,0.066125));
#5745=CARTESIAN_POINT('',(0.04655,-0.0122,0.066125));
#5746=CARTESIAN_POINT('',(0.04655,-0.009975,0.066125));
#5747=CARTESIAN_POINT('',(0.06655,-0.0122,0.066125));
#5748=CARTESIAN_POINT('Origin',(0.06655,-0.00275,0.02565));
#5749=CARTESIAN_POINT('',(0.06855,-0.00275,0.061125));
#5750=CARTESIAN_POINT('',(0.06855,-0.00275,-0.009825));
#5751=CARTESIAN_POINT('',(0.06855,-0.00275,0.02565));
#5752=CARTESIAN_POINT('',(0.04655,-0.00275,-0.009825));
#5753=CARTESIAN_POINT('',(0.06655,-0.00275,-0.009825));
#5754=CARTESIAN_POINT('',(0.04655,-0.00275,0.061125));
#5755=CARTESIAN_POINT('',(0.04655,-0.00275,0.02565));
#5756=CARTESIAN_POINT('',(0.04655,-0.00275,0.061125));
#5757=CARTESIAN_POINT('',(0.05755,-0.00275,0.0218));
#5758=CARTESIAN_POINT('Origin',(0.05755,-0.00275,0.014175));
#5759=CARTESIAN_POINT('',(0.05755,-0.00275,0.04475));
#5760=CARTESIAN_POINT('Origin',(0.05755,-0.00275,0.037125));
#5761=CARTESIAN_POINT('Origin',(0.06655,-0.009975,-0.014825));
#5762=CARTESIAN_POINT('',(0.06855,-0.00775,-0.014825));
#5763=CARTESIAN_POINT('',(0.06855,-0.0122,-0.014825));
#5764=CARTESIAN_POINT('',(0.06855,-0.009975,-0.014825));
#5765=CARTESIAN_POINT('',(0.04655,-0.0122,-0.014825));
#5766=CARTESIAN_POINT('',(0.06855,-0.0122,-0.014825));
#5767=CARTESIAN_POINT('',(0.04655,-0.00775,-0.014825));
#5768=CARTESIAN_POINT('',(0.04655,-0.009975,-0.014825));
#5769=CARTESIAN_POINT('',(0.06655,-0.00775,-0.014825));
#5770=CARTESIAN_POINT('Origin',(0.06655,-0.009975,-0.0076));
#5771=CARTESIAN_POINT('',(0.06655,-0.009975,-0.003375));
#5772=CARTESIAN_POINT('Origin',(0.06655,-0.009975,-0.0076));
#5773=CARTESIAN_POINT('',(0.04655,-0.009975,-0.003375));
#5774=CARTESIAN_POINT('',(0.06655,-0.009975,-0.003375));
#5775=CARTESIAN_POINT('Origin',(0.04655,-0.009975,-0.0076));
#5776=CARTESIAN_POINT('Origin',(0.06655,-0.0172,0.02565));
#5777=CARTESIAN_POINT('',(0.06855,-0.0172,0.061125));
#5778=CARTESIAN_POINT('',(0.06855,-0.0172,0.053125));
#5779=CARTESIAN_POINT('',(0.06855,-0.0172,0.02565));
#5780=CARTESIAN_POINT('',(0.04655,-0.0172,0.061125));
#5781=CARTESIAN_POINT('',(0.06655,-0.0172,0.061125));
#5782=CARTESIAN_POINT('',(0.04655,-0.0172,0.053125));
#5783=CARTESIAN_POINT('',(0.04655,-0.0172,0.02565));
#5784=CARTESIAN_POINT('',(0.04655,-0.0172,0.053125));
#5785=CARTESIAN_POINT('Origin',(0.06655,-0.01,0.0589));
#5786=CARTESIAN_POINT('',(0.06655,-0.01,0.063125));
#5787=CARTESIAN_POINT('Origin',(0.06655,-0.01,0.0589));
#5788=CARTESIAN_POINT('',(0.04655,-0.01,0.063125));
#5789=CARTESIAN_POINT('',(0.06655,-0.01,0.063125));
#5790=CARTESIAN_POINT('Origin',(0.04655,-0.01,0.0589));
#5791=CARTESIAN_POINT('Origin',(0.04655,0.,0.02565));
#5792=CARTESIAN_POINT('',(0.04655,-0.0272,0.043125));
#5793=CARTESIAN_POINT('',(0.04655,-0.0272,0.008175));
#5794=CARTESIAN_POINT('',(0.04655,-0.0272,0.02565));
#5795=CARTESIAN_POINT('',(0.04655,-0.0222,0.048125));
#5796=CARTESIAN_POINT('Origin',(0.04655,-0.0222,0.043125));
#5797=CARTESIAN_POINT('Origin',(0.04655,-0.0222,0.053125));
#5798=CARTESIAN_POINT('Origin',(0.04655,-0.0122,0.061125));
#5799=CARTESIAN_POINT('Origin',(0.04655,-0.00775,0.061125));
#5800=CARTESIAN_POINT('Origin',(0.04655,-0.00775,-0.009825));
#5801=CARTESIAN_POINT('Origin',(0.04655,-0.0122,-0.009825));
#5802=CARTESIAN_POINT('',(0.04655,-0.0222,0.003175));
#5803=CARTESIAN_POINT('Origin',(0.04655,-0.0222,-0.001825));
#5804=CARTESIAN_POINT('Origin',(0.04655,-0.0222,0.008175));
#5805=CARTESIAN_POINT('Origin',(0.06655,-0.009975,0.02565));
#5806=CARTESIAN_POINT('Origin',(0.06655,-0.009975,0.02565));
#5807=CARTESIAN_POINT('Origin',(0.06855,-0.009975,0.02565));
#5808=CARTESIAN_POINT('Origin',(0.06855,-0.0122,-0.009825));
#5809=CARTESIAN_POINT('Origin',(0.06855,-0.00775,-0.009825));
#5810=CARTESIAN_POINT('Origin',(0.06855,-0.00775,0.061125));
#5811=CARTESIAN_POINT('Origin',(0.06855,-0.0122,0.061125));
#5812=CARTESIAN_POINT('',(0.06855,-0.0222,0.048125));
#5813=CARTESIAN_POINT('Origin',(0.06855,-0.0222,0.053125));
#5814=CARTESIAN_POINT('',(0.06855,-0.0272,0.043125));
#5815=CARTESIAN_POINT('Origin',(0.06855,-0.0222,0.043125));
#5816=CARTESIAN_POINT('',(0.06855,-0.0272,0.008175));
#5817=CARTESIAN_POINT('',(0.06855,-0.0272,0.02565));
#5818=CARTESIAN_POINT('',(0.06855,-0.0222,0.003175));
#5819=CARTESIAN_POINT('Origin',(0.06855,-0.0222,0.008175));
#5820=CARTESIAN_POINT('Origin',(0.06855,-0.0222,-0.001825));
#5821=CARTESIAN_POINT('Origin',(0.06655,-0.0122,0.061125));
#5822=CARTESIAN_POINT('Origin',(0.06655,-0.00775,0.061125));
#5823=CARTESIAN_POINT('Origin',(0.06655,-0.00775,-0.009825));
#5824=CARTESIAN_POINT('Origin',(0.06655,-0.0122,-0.009825));
#5825=CARTESIAN_POINT('Origin',(0.05755,-0.0272,0.02565));
#5826=CARTESIAN_POINT('',(0.0622553825561797,-0.0272,0.043125));
#5827=CARTESIAN_POINT('',(0.05755,-0.0272,0.043125));
#5828=CARTESIAN_POINT('',(0.0528446174438203,-0.0272,0.043125));
#5829=CARTESIAN_POINT('Origin',(0.05755,-0.0272,0.037125));
#5830=CARTESIAN_POINT('',(0.05755,-0.0272,0.043125));
#5831=CARTESIAN_POINT('',(0.0528446174438203,-0.0272,0.008175));
#5832=CARTESIAN_POINT('',(0.04655,-0.0272,0.008175));
#5833=CARTESIAN_POINT('',(0.05755,-0.0272,0.0218));
#5834=CARTESIAN_POINT('Origin',(0.05755,-0.0272,0.014175));
#5835=CARTESIAN_POINT('',(0.0622553825561797,-0.0272,0.008175));
#5836=CARTESIAN_POINT('Origin',(0.05755,-0.0272,0.014175));
#5837=CARTESIAN_POINT('',(0.04655,-0.0272,0.008175));
#5838=CARTESIAN_POINT('Origin',(0.05755,-0.0022,0.037125));
#5839=CARTESIAN_POINT('',(0.05755,-0.0269285700798444,0.04475));
#5840=CARTESIAN_POINT('',(0.05755,-0.0022,0.04475));
#5841=CARTESIAN_POINT('Ctrl Pts',(0.0528446174438203,-0.0272,0.043125));
#5842=CARTESIAN_POINT('Ctrl Pts',(0.0533814087034594,-0.0272,0.0435459680382359));
#5843=CARTESIAN_POINT('Ctrl Pts',(0.0539899057191737,-0.027146490983882,
0.0439040351600042));
#5844=CARTESIAN_POINT('Ctrl Pts',(0.0555707240629267,-0.0270066019492738,
0.0445577665669935));
#5845=CARTESIAN_POINT('Ctrl Pts',(0.056588612994316,-0.0269285700798444,
0.04475));
#5846=CARTESIAN_POINT('Ctrl Pts',(0.05755,-0.0269285700798444,0.04475));
#5847=CARTESIAN_POINT('Ctrl Pts',(0.05755,-0.0269285700798444,0.04475));
#5848=CARTESIAN_POINT('Ctrl Pts',(0.058511387005684,-0.0269285700798444,
0.04475));
#5849=CARTESIAN_POINT('Ctrl Pts',(0.0595292759370733,-0.0270066019492738,
0.0445577665669935));
#5850=CARTESIAN_POINT('Ctrl Pts',(0.0611100942808263,-0.027146490983882,
0.0439040351600042));
#5851=CARTESIAN_POINT('Ctrl Pts',(0.0617185912965407,-0.0272,0.0435459680382359));
#5852=CARTESIAN_POINT('Ctrl Pts',(0.0622553825561797,-0.0272,0.043125));
#5853=CARTESIAN_POINT('Origin',(0.05755,-0.0022,0.014175));
#5854=CARTESIAN_POINT('',(0.05755,-0.0022,0.0218));
#5855=CARTESIAN_POINT('Ctrl Pts',(0.0622553825561797,-0.0272,0.00817500000000001));
#5856=CARTESIAN_POINT('Ctrl Pts',(0.0617185912965407,-0.0272,0.00775403196176415));
#5857=CARTESIAN_POINT('Ctrl Pts',(0.0611100942808263,-0.027146490983882,
0.00739596483999584));
#5858=CARTESIAN_POINT('Ctrl Pts',(0.0595292759370733,-0.0270066019492738,
0.00674223343300649));
#5859=CARTESIAN_POINT('Ctrl Pts',(0.058511387005684,-0.0269285700798444,
0.00655));
#5860=CARTESIAN_POINT('Ctrl Pts',(0.056588612994316,-0.0269285700798444,
0.00655));
#5861=CARTESIAN_POINT('Ctrl Pts',(0.0555707240629267,-0.0270066019492738,
0.00674223343300649));
#5862=CARTESIAN_POINT('Ctrl Pts',(0.0539899057191737,-0.027146490983882,
0.00739596483999584));
#5863=CARTESIAN_POINT('Ctrl Pts',(0.0533814087034593,-0.0272,0.00775403196176414));
#5864=CARTESIAN_POINT('Ctrl Pts',(0.0528446174438203,-0.0272,0.00817500000000001));
#5865=CARTESIAN_POINT('Origin',(0.05755,-0.0222,0.008175));
#5866=CARTESIAN_POINT('',(0.06855,-0.0222,0.003175));
#5867=CARTESIAN_POINT('Origin',(0.05755,-0.0222,-0.001825));
#5868=CARTESIAN_POINT('Origin',(0.05755,-0.0222,0.043125));
#5869=CARTESIAN_POINT('',(0.05755,-0.0222,0.048125));
#5870=CARTESIAN_POINT('Origin',(0.06655,-0.0222,0.053125));
#5871=CARTESIAN_POINT('',(0.,0.,0.));
#5872=CARTESIAN_POINT('Origin',(-0.06655,-0.0172,0.02565));
#5873=CARTESIAN_POINT('',(-0.04655,-0.0172,-0.001825));
#5874=CARTESIAN_POINT('',(-0.04655,-0.0172,-0.009825));
#5875=CARTESIAN_POINT('',(-0.04655,-0.0172,0.02565));
#5876=CARTESIAN_POINT('',(-0.06855,-0.0172,-0.001825));
#5877=CARTESIAN_POINT('',(-0.06655,-0.0172,-0.001825));
#5878=CARTESIAN_POINT('',(-0.06855,-0.0172,-0.009825));
#5879=CARTESIAN_POINT('',(-0.06855,-0.0172,0.02565));
#5880=CARTESIAN_POINT('',(-0.04655,-0.0172,-0.009825));
#5881=CARTESIAN_POINT('Origin',(-0.06655,-0.009975,0.066125));
#5882=CARTESIAN_POINT('',(-0.06855,-0.00775,0.066125));
#5883=CARTESIAN_POINT('',(-0.06855,-0.0122,0.066125));
#5884=CARTESIAN_POINT('',(-0.06855,-0.009975,0.066125));
#5885=CARTESIAN_POINT('',(-0.04655,-0.0122,0.066125));
#5886=CARTESIAN_POINT('',(-0.06655,-0.0122,0.066125));
#5887=CARTESIAN_POINT('',(-0.04655,-0.00775,0.066125));
#5888=CARTESIAN_POINT('',(-0.04655,-0.009975,0.066125));
#5889=CARTESIAN_POINT('',(-0.06855,-0.00775,0.066125));
#5890=CARTESIAN_POINT('Origin',(-0.06655,-0.00275,0.02565));
#5891=CARTESIAN_POINT('',(-0.06855,-0.00275,0.061125));
#5892=CARTESIAN_POINT('',(-0.06855,-0.00275,-0.009825));
#5893=CARTESIAN_POINT('',(-0.06855,-0.00275,0.02565));
#5894=CARTESIAN_POINT('',(-0.04655,-0.00275,0.061125));
#5895=CARTESIAN_POINT('',(-0.04655,-0.00275,0.061125));
#5896=CARTESIAN_POINT('',(-0.04655,-0.00275,-0.009825));
#5897=CARTESIAN_POINT('',(-0.04655,-0.00275,0.02565));
#5898=CARTESIAN_POINT('',(-0.06655,-0.00275,-0.009825));
#5899=CARTESIAN_POINT('',(-0.05755,-0.00275,0.0218));
#5900=CARTESIAN_POINT('Origin',(-0.05755,-0.00275,0.014175));
#5901=CARTESIAN_POINT('',(-0.05755,-0.00275,0.04475));
#5902=CARTESIAN_POINT('Origin',(-0.05755,-0.00275,0.037125));
#5903=CARTESIAN_POINT('Origin',(-0.06655,-0.009975,-0.014825));
#5904=CARTESIAN_POINT('',(-0.06855,-0.00775,-0.014825));
#5905=CARTESIAN_POINT('',(-0.06855,-0.0122,-0.014825));
#5906=CARTESIAN_POINT('',(-0.06855,-0.009975,-0.014825));
#5907=CARTESIAN_POINT('',(-0.04655,-0.00775,-0.014825));
#5908=CARTESIAN_POINT('',(-0.06655,-0.00775,-0.014825));
#5909=CARTESIAN_POINT('',(-0.04655,-0.0122,-0.014825));
#5910=CARTESIAN_POINT('',(-0.04655,-0.009975,-0.014825));
#5911=CARTESIAN_POINT('',(-0.06855,-0.0122,-0.014825));
#5912=CARTESIAN_POINT('Origin',(-0.06655,-0.009975,-0.0076));
#5913=CARTESIAN_POINT('',(-0.06655,-0.009975,-0.003375));
#5914=CARTESIAN_POINT('Origin',(-0.06655,-0.009975,-0.0076));
#5915=CARTESIAN_POINT('',(-0.04655,-0.009975,-0.003375));
#5916=CARTESIAN_POINT('',(-0.06655,-0.009975,-0.003375));
#5917=CARTESIAN_POINT('Origin',(-0.04655,-0.009975,-0.0076));
#5918=CARTESIAN_POINT('Origin',(-0.06655,-0.0172,0.02565));
#5919=CARTESIAN_POINT('',(-0.06855,-0.0172,0.061125));
#5920=CARTESIAN_POINT('',(-0.06855,-0.0172,0.053125));
#5921=CARTESIAN_POINT('',(-0.06855,-0.0172,0.02565));
#5922=CARTESIAN_POINT('',(-0.04655,-0.0172,0.053125));
#5923=CARTESIAN_POINT('',(-0.04655,-0.0172,0.053125));
#5924=CARTESIAN_POINT('',(-0.04655,-0.0172,0.061125));
#5925=CARTESIAN_POINT('',(-0.04655,-0.0172,0.02565));
#5926=CARTESIAN_POINT('',(-0.06655,-0.0172,0.061125));
#5927=CARTESIAN_POINT('Origin',(-0.06655,-0.01,0.0589));
#5928=CARTESIAN_POINT('',(-0.06655,-0.01,0.063125));
#5929=CARTESIAN_POINT('Origin',(-0.06655,-0.01,0.0589));
#5930=CARTESIAN_POINT('',(-0.04655,-0.01,0.063125));
#5931=CARTESIAN_POINT('',(-0.06655,-0.01,0.063125));
#5932=CARTESIAN_POINT('Origin',(-0.04655,-0.01,0.0589));
#5933=CARTESIAN_POINT('Origin',(-0.04655,0.,0.02565));
#5934=CARTESIAN_POINT('',(-0.04655,-0.0272,0.043125));
#5935=CARTESIAN_POINT('',(-0.04655,-0.0272,0.008175));
#5936=CARTESIAN_POINT('',(-0.04655,-0.0272,0.02565));
#5937=CARTESIAN_POINT('',(-0.04655,-0.0222,0.003175));
#5938=CARTESIAN_POINT('Origin',(-0.04655,-0.0222,0.008175));
#5939=CARTESIAN_POINT('Origin',(-0.04655,-0.0222,-0.001825));
#5940=CARTESIAN_POINT('Origin',(-0.04655,-0.0122,-0.009825));
#5941=CARTESIAN_POINT('Origin',(-0.04655,-0.00775,-0.009825));
#5942=CARTESIAN_POINT('Origin',(-0.04655,-0.00775,0.061125));
#5943=CARTESIAN_POINT('Origin',(-0.04655,-0.0122,0.061125));
#5944=CARTESIAN_POINT('',(-0.04655,-0.0222,0.048125));
#5945=CARTESIAN_POINT('Origin',(-0.04655,-0.0222,0.053125));
#5946=CARTESIAN_POINT('Origin',(-0.04655,-0.0222,0.043125));
#5947=CARTESIAN_POINT('Origin',(-0.06655,-0.009975,0.02565));
#5948=CARTESIAN_POINT('Origin',(-0.06655,-0.009975,0.02565));
#5949=CARTESIAN_POINT('Origin',(-0.06855,-0.009975,0.02565));
#5950=CARTESIAN_POINT('',(-0.06855,-0.0222,0.003175));
#5951=CARTESIAN_POINT('Origin',(-0.06855,-0.0222,-0.001825));
#5952=CARTESIAN_POINT('',(-0.06855,-0.0272,0.008175));
#5953=CARTESIAN_POINT('Origin',(-0.06855,-0.0222,0.008175));
#5954=CARTESIAN_POINT('',(-0.06855,-0.0272,0.043125));
#5955=CARTESIAN_POINT('',(-0.06855,-0.0272,0.02565));
#5956=CARTESIAN_POINT('',(-0.06855,-0.0222,0.048125));
#5957=CARTESIAN_POINT('Origin',(-0.06855,-0.0222,0.043125));
#5958=CARTESIAN_POINT('Origin',(-0.06855,-0.0222,0.053125));
#5959=CARTESIAN_POINT('Origin',(-0.06855,-0.0122,0.061125));
#5960=CARTESIAN_POINT('Origin',(-0.06855,-0.00775,0.061125));
#5961=CARTESIAN_POINT('Origin',(-0.06855,-0.00775,-0.009825));
#5962=CARTESIAN_POINT('Origin',(-0.06855,-0.0122,-0.009825));
#5963=CARTESIAN_POINT('Origin',(-0.06655,-0.0122,0.061125));
#5964=CARTESIAN_POINT('Origin',(-0.06655,-0.00775,0.061125));
#5965=CARTESIAN_POINT('Origin',(-0.06655,-0.00775,-0.009825));
#5966=CARTESIAN_POINT('Origin',(-0.06655,-0.0122,-0.009825));
#5967=CARTESIAN_POINT('Origin',(-0.05755,-0.0272,0.02565));
#5968=CARTESIAN_POINT('',(-0.0622553825561797,-0.0272,0.008175));
#5969=CARTESIAN_POINT('',(-0.04655,-0.0272,0.008175));
#5970=CARTESIAN_POINT('',(-0.05755,-0.0272,0.0218));
#5971=CARTESIAN_POINT('Origin',(-0.05755,-0.0272,0.014175));
#5972=CARTESIAN_POINT('',(-0.0528446174438203,-0.0272,0.008175));
#5973=CARTESIAN_POINT('Origin',(-0.05755,-0.0272,0.014175));
#5974=CARTESIAN_POINT('',(-0.04655,-0.0272,0.008175));
#5975=CARTESIAN_POINT('',(-0.0528446174438203,-0.0272,0.043125));
#5976=CARTESIAN_POINT('',(-0.05755,-0.0272,0.043125));
#5977=CARTESIAN_POINT('',(-0.0622553825561797,-0.0272,0.043125));
#5978=CARTESIAN_POINT('Origin',(-0.05755,-0.0272,0.037125));
#5979=CARTESIAN_POINT('',(-0.05755,-0.0272,0.043125));
#5980=CARTESIAN_POINT('Origin',(-0.05755,-0.0022,0.037125));
#5981=CARTESIAN_POINT('',(-0.05755,-0.0269285700798444,0.04475));
#5982=CARTESIAN_POINT('',(-0.05755,-0.0022,0.04475));
#5983=CARTESIAN_POINT('Ctrl Pts',(-0.0622553825561797,-0.0272,0.043125));
#5984=CARTESIAN_POINT('Ctrl Pts',(-0.0617185912965407,-0.0272,0.0435459680382359));
#5985=CARTESIAN_POINT('Ctrl Pts',(-0.0611100942808263,-0.027146490983882,
0.0439040351600042));
#5986=CARTESIAN_POINT('Ctrl Pts',(-0.0595292759370733,-0.0270066019492738,
0.0445577665669935));
#5987=CARTESIAN_POINT('Ctrl Pts',(-0.058511387005684,-0.0269285700798444,
0.04475));
#5988=CARTESIAN_POINT('Ctrl Pts',(-0.05755,-0.0269285700798444,0.04475));
#5989=CARTESIAN_POINT('Ctrl Pts',(-0.05755,-0.0269285700798444,0.04475));
#5990=CARTESIAN_POINT('Ctrl Pts',(-0.056588612994316,-0.0269285700798444,
0.04475));
#5991=CARTESIAN_POINT('Ctrl Pts',(-0.0555707240629267,-0.0270066019492738,
0.0445577665669935));
#5992=CARTESIAN_POINT('Ctrl Pts',(-0.0539899057191737,-0.027146490983882,
0.0439040351600042));
#5993=CARTESIAN_POINT('Ctrl Pts',(-0.0533814087034593,-0.0272,0.0435459680382359));
#5994=CARTESIAN_POINT('Ctrl Pts',(-0.0528446174438203,-0.0272,0.043125));
#5995=CARTESIAN_POINT('Origin',(-0.05755,-0.0022,0.014175));
#5996=CARTESIAN_POINT('',(-0.05755,-0.0022,0.0218));
#5997=CARTESIAN_POINT('Ctrl Pts',(-0.0622553825561797,-0.0272,0.00817500000000001));
#5998=CARTESIAN_POINT('Ctrl Pts',(-0.0617185912965407,-0.0272,0.00775403196176415));
#5999=CARTESIAN_POINT('Ctrl Pts',(-0.0611100942808263,-0.027146490983882,
0.00739596483999584));
#6000=CARTESIAN_POINT('Ctrl Pts',(-0.0595292759370733,-0.0270066019492738,
0.00674223343300649));
#6001=CARTESIAN_POINT('Ctrl Pts',(-0.058511387005684,-0.0269285700798444,
0.00655));
#6002=CARTESIAN_POINT('Ctrl Pts',(-0.056588612994316,-0.0269285700798444,
0.00655));
#6003=CARTESIAN_POINT('Ctrl Pts',(-0.0555707240629267,-0.0270066019492738,
0.00674223343300649));
#6004=CARTESIAN_POINT('Ctrl Pts',(-0.0539899057191737,-0.027146490983882,
0.00739596483999584));
#6005=CARTESIAN_POINT('Ctrl Pts',(-0.0533814087034593,-0.0272,0.00775403196176415));
#6006=CARTESIAN_POINT('Ctrl Pts',(-0.0528446174438203,-0.0272,0.00817500000000001));
#6007=CARTESIAN_POINT('Origin',(-0.05755,-0.0222,0.008175));
#6008=CARTESIAN_POINT('',(-0.06855,-0.0222,0.003175));
#6009=CARTESIAN_POINT('Origin',(-0.05755,-0.0222,-0.001825));
#6010=CARTESIAN_POINT('Origin',(-0.05755,-0.0222,0.043125));
#6011=CARTESIAN_POINT('',(-0.05755,-0.0222,0.048125));
#6012=CARTESIAN_POINT('Origin',(-0.06655,-0.0222,0.053125));
#6013=CARTESIAN_POINT('',(0.,0.,0.));
#6014=CARTESIAN_POINT('Origin',(0.,2.4492935982947E-19,0.265));
#6015=CARTESIAN_POINT('',(-0.004,-2.44929359829471E-19,0.0015));
#6016=CARTESIAN_POINT('',(0.004,-2.44929359829471E-19,0.00149999999999999));
#6017=CARTESIAN_POINT('Origin',(0.,2.4492935982947E-19,0.0015));
#6018=CARTESIAN_POINT('',(0.004,-2.44929359829471E-19,0.2635));
#6019=CARTESIAN_POINT('',(0.004,-2.44929359829471E-19,0.265));
#6020=CARTESIAN_POINT('',(-0.004,-2.44929359829471E-19,0.2635));
#6021=CARTESIAN_POINT('Origin',(0.,2.4492935982947E-19,0.2635));
#6022=CARTESIAN_POINT('Origin',(0.,2.4492935982947E-19,0.2635));
#6023=CARTESIAN_POINT('Origin',(0.,2.4492935982947E-19,0.0015));
#6024=CARTESIAN_POINT('Origin',(0.,0.,0.265));
#6025=CARTESIAN_POINT('',(-0.0025,-6.12323399573683E-20,0.265));
#6026=CARTESIAN_POINT('Origin',(0.,2.4492935982947E-19,0.265));
#6027=CARTESIAN_POINT('Origin',(0.,0.,0.));
#6028=CARTESIAN_POINT('',(-0.0025,-6.12323399573683E-20,0.));
#6029=CARTESIAN_POINT('Origin',(0.,2.4492935982947E-19,0.));
#6030=CARTESIAN_POINT('Origin',(0.,2.4492935982947E-19,0.0015));
#6031=CARTESIAN_POINT('Origin',(-0.0025,-6.12323399573683E-20,0.0015));
#6032=CARTESIAN_POINT('Origin',(0.,2.4492935982947E-19,0.2635));
#6033=CARTESIAN_POINT('Origin',(-0.0025,-6.12323399573683E-20,0.2635));
#6034=CARTESIAN_POINT('',(0.,0.,0.));
#6035=CARTESIAN_POINT('',(0.,0.,0.));
#6036=CARTESIAN_POINT('',(0.,0.,0.));
#6037=CARTESIAN_POINT('',(0.,0.,0.));
#6038=CARTESIAN_POINT('',(0.,0.,0.));
#6039=CARTESIAN_POINT('',(0.,0.,0.));
#6040=CARTESIAN_POINT('',(0.,0.,0.));
#6041=CARTESIAN_POINT('',(0.,0.,0.));
#6042=CARTESIAN_POINT('',(0.,0.,0.));
#6043=CARTESIAN_POINT('',(0.,0.,0.));
#6044=CARTESIAN_POINT('',(0.,0.,0.));
#6045=CARTESIAN_POINT('',(0.,0.,0.));
#6046=CARTESIAN_POINT('Origin',(0.,-0.0119,0.));
#6047=CARTESIAN_POINT('',(0.,-0.01180000000001,-0.00650000000001));
#6048=CARTESIAN_POINT('',(-7.96020419447004E-19,-0.01180000000001,0.00650000000001));
#6049=CARTESIAN_POINT('Origin',(0.,-0.01180000000001,0.));
#6050=CARTESIAN_POINT('',(-8.20513355429951E-19,-0.01200000000001,0.00670000000001));
#6051=CARTESIAN_POINT('',(-8.08266887437253E-19,-0.0119,0.0066));
#6052=CARTESIAN_POINT('Origin',(0.,-0.01200000000001,0.));
#6053=CARTESIAN_POINT('Origin',(0.,-0.01180000000001,0.));
#6054=CARTESIAN_POINT('Origin',(0.,-0.012,0.0075));
#6055=CARTESIAN_POINT('',(8.93992163377568E-19,-0.012,0.0073));
#6056=CARTESIAN_POINT('Origin',(0.,-0.01200000000001,0.));
#6057=CARTESIAN_POINT('Origin',(0.,-0.0115000000819564,0.));
#6058=CARTESIAN_POINT('',(-7.9602041944578E-19,-0.0110000001639228,-0.0065));
#6059=CARTESIAN_POINT('',(-7.9602041944578E-19,-0.0115000000819564,-0.0065));
#6060=CARTESIAN_POINT('Origin',(0.,-0.0110000001639228,0.));
#6061=CARTESIAN_POINT('Origin',(0.,-0.0119,0.));
#6062=CARTESIAN_POINT('',(0.,-0.01180000000001,-0.00750000000001));
#6063=CARTESIAN_POINT('',(9.18485099360515E-19,-0.0118,0.0075));
#6064=CARTESIAN_POINT('Origin',(0.,-0.01180000000001,0.));
#6065=CARTESIAN_POINT('',(9.06238631369041E-19,-0.0119,0.0074));
#6066=CARTESIAN_POINT('Origin',(0.,-0.01180000000001,0.));
#6067=CARTESIAN_POINT('Origin',(0.,-0.010375,0.));
#6068=CARTESIAN_POINT('',(-9.18485099360515E-19,-0.00875000000001,-0.0075));
#6069=CARTESIAN_POINT('Origin',(0.,-0.00875000000001,0.));
#6070=CARTESIAN_POINT('',(-9.18485099360515E-19,-0.010375,-0.0075));
#6071=CARTESIAN_POINT('Origin',(0.,0.0119,0.));
#6072=CARTESIAN_POINT('',(0.,0.01180000000001,-0.00650000000001));
#6073=CARTESIAN_POINT('',(7.96020419447004E-19,0.01180000000001,0.00650000000001));
#6074=CARTESIAN_POINT('Origin',(0.,0.01180000000001,0.));
#6075=CARTESIAN_POINT('',(8.20513355429951E-19,0.01200000000001,0.00670000000001));
#6076=CARTESIAN_POINT('',(8.08266887437253E-19,0.0119,0.0066));
#6077=CARTESIAN_POINT('Origin',(0.,0.01200000000001,0.));
#6078=CARTESIAN_POINT('Origin',(0.,0.01180000000001,0.));
#6079=CARTESIAN_POINT('Origin',(0.,0.012,0.0065));
#6080=CARTESIAN_POINT('',(-8.93992163377568E-19,0.012,0.0073));
#6081=CARTESIAN_POINT('Origin',(0.,0.01200000000001,0.));
#6082=CARTESIAN_POINT('Origin',(0.,0.0115000000819564,0.));
#6083=CARTESIAN_POINT('',(-7.9602041944578E-19,0.0110000001639228,-0.0065));
#6084=CARTESIAN_POINT('Origin',(0.,0.0110000001639228,0.));
#6085=CARTESIAN_POINT('',(-7.9602041944578E-19,0.0115000000819564,-0.0065));
#6086=CARTESIAN_POINT('Origin',(0.,0.0119,0.));
#6087=CARTESIAN_POINT('',(0.,0.01180000000001,-0.00750000000001));
#6088=CARTESIAN_POINT('',(-9.18485099360515E-19,0.0118,0.0075));
#6089=CARTESIAN_POINT('Origin',(0.,0.01180000000001,0.));
#6090=CARTESIAN_POINT('',(-9.06238631369041E-19,0.0119,0.0074));
#6091=CARTESIAN_POINT('Origin',(0.,0.01180000000001,0.));
#6092=CARTESIAN_POINT('Origin',(0.,0.010375,0.));
#6093=CARTESIAN_POINT('',(-9.18485099360515E-19,0.00875000000001,-0.0075));
#6094=CARTESIAN_POINT('',(-9.18485099360515E-19,0.010375,-0.0075));
#6095=CARTESIAN_POINT('Origin',(0.,0.00875000000001,0.));
#6096=CARTESIAN_POINT('Origin',(0.,0.0110000001639128,0.00700000010430813));
#6097=CARTESIAN_POINT('',(-8.57252772177209E-19,0.0110000001639228,-0.00700000010430813));
#6098=CARTESIAN_POINT('Origin',(0.,0.0110000001639228,0.));
#6099=CARTESIAN_POINT('Origin',(0.,0.0107500001601875,0.));
#6100=CARTESIAN_POINT('',(-8.57252772177209E-19,0.0105000001564722,-0.00700000010430813));
#6101=CARTESIAN_POINT('Origin',(0.,0.0105000001564722,0.));
#6102=CARTESIAN_POINT('',(-8.57252772177209E-19,0.0107500001601875,-0.00700000010430813));
#6103=CARTESIAN_POINT('Origin',(0.,0.0105000001564622,0.0063));
#6104=CARTESIAN_POINT('',(-7.71527483462833E-19,0.0105000001564722,-0.0063));
#6105=CARTESIAN_POINT('Origin',(0.,0.0105000001564722,0.));
#6106=CARTESIAN_POINT('Origin',(0.,0.0093500000782311,0.));
#6107=CARTESIAN_POINT('',(-7.71527483462833E-19,0.00820000000001,-0.0063));
#6108=CARTESIAN_POINT('Origin',(0.,0.00820000000001,0.));
#6109=CARTESIAN_POINT('',(-7.71527483462833E-19,0.0093500000782311,-0.0063));
#6110=CARTESIAN_POINT('Origin',(0.,0.00695,0.));
#6111=CARTESIAN_POINT('',(-7.2254161149716E-19,0.00570000000001131,-0.00590000000000181));
#6112=CARTESIAN_POINT('Origin',(0.,0.00570000000001,0.));
#6113=CARTESIAN_POINT('',(-7.47034547479885E-19,0.00695,-0.0061));
#6114=CARTESIAN_POINT('Origin',(0.,0.,0.));
#6115=CARTESIAN_POINT('',(-7.22541611496938E-19,-0.00570000000001,-0.0059));
#6116=CARTESIAN_POINT('Origin',(0.,-0.00570000000001,0.));
#6117=CARTESIAN_POINT('',(-7.22541611496938E-19,0.,-0.0059));
#6118=CARTESIAN_POINT('Origin',(0.,-0.00695,0.));
#6119=CARTESIAN_POINT('',(7.71527483463054E-19,-0.00820000000001131,-0.00630000000000181));
#6120=CARTESIAN_POINT('',(7.47034547479885E-19,-0.00695,-0.0061));
#6121=CARTESIAN_POINT('Origin',(0.,-0.00820000000001,0.));
#6122=CARTESIAN_POINT('Origin',(0.,-0.0093500000782311,0.));
#6123=CARTESIAN_POINT('',(-7.71527483462833E-19,-0.0105000001564722,-0.0063));
#6124=CARTESIAN_POINT('Origin',(0.,-0.0105000001564722,0.));
#6125=CARTESIAN_POINT('',(-7.71527483462833E-19,-0.0093500000782311,-0.0063));
#6126=CARTESIAN_POINT('Origin',(0.,-0.0105000001564622,0.00700000010430813));
#6127=CARTESIAN_POINT('',(-8.57252772177209E-19,-0.0105000001564722,-0.00700000010430813));
#6128=CARTESIAN_POINT('Origin',(0.,-0.0105000001564722,0.));
#6129=CARTESIAN_POINT('Origin',(0.,-0.0107500001601875,0.));
#6130=CARTESIAN_POINT('',(-8.57252772177209E-19,-0.0110000001639228,-0.00700000010430813));
#6131=CARTESIAN_POINT('Origin',(0.,-0.0110000001639228,0.));
#6132=CARTESIAN_POINT('',(-8.57252772177209E-19,-0.0107500001601875,-0.00700000010430813));
#6133=CARTESIAN_POINT('Origin',(0.,-0.0110000001639128,0.0065));
#6134=CARTESIAN_POINT('Origin',(0.,-0.00875,0.00715));
#6135=CARTESIAN_POINT('',(-8.75622461390357E-19,-0.00875000000001,-0.00715));
#6136=CARTESIAN_POINT('Origin',(0.,-0.00875000000001,0.));
#6137=CARTESIAN_POINT('Origin',(0.,-0.0082,0.));
#6138=CARTESIAN_POINT('',(-8.75622461390357E-19,-0.00765000000001,-0.00715));
#6139=CARTESIAN_POINT('Origin',(0.,-0.00765000000001,0.));
#6140=CARTESIAN_POINT('',(-8.75622461390357E-19,-0.0082,-0.00715));
#6141=CARTESIAN_POINT('Origin',(0.,-0.00765,0.0075));
#6142=CARTESIAN_POINT('',(-9.18485099360515E-19,-0.00765000000001,-0.0075));
#6143=CARTESIAN_POINT('Origin',(0.,-0.00765000000001,0.));
#6144=CARTESIAN_POINT('Origin',(0.,0.,0.));
#6145=CARTESIAN_POINT('',(-9.18485099360515E-19,0.00765000000001,-0.0075));
#6146=CARTESIAN_POINT('Origin',(0.,0.00765000000001,0.));
#6147=CARTESIAN_POINT('',(-9.18485099360515E-19,0.,-0.0075));
#6148=CARTESIAN_POINT('Origin',(0.,0.00765,0.00715));
#6149=CARTESIAN_POINT('',(-8.75622461390357E-19,0.00765000000001,-0.00715));
#6150=CARTESIAN_POINT('Origin',(0.,0.00765000000001,0.));
#6151=CARTESIAN_POINT('Origin',(0.,0.0082,0.));
#6152=CARTESIAN_POINT('',(-8.75622461390357E-19,0.00875000000001,-0.00715));
#6153=CARTESIAN_POINT('Origin',(0.,0.00875000000001,0.));
#6154=CARTESIAN_POINT('',(-8.75622461390357E-19,0.0082,-0.00715));
#6155=CARTESIAN_POINT('Origin',(0.,0.00875,0.0075));
#6156=CARTESIAN_POINT('',(0.,0.,0.));
#6157=CARTESIAN_POINT('Origin',(0.,0.0116999997384846,0.0065));
#6158=CARTESIAN_POINT('',(-7.9602041944578E-19,0.0116999997384946,-0.0065));
#6159=CARTESIAN_POINT('Origin',(0.,0.0116999997384946,0.));
#6160=CARTESIAN_POINT('',(5.87830450451699E-19,0.0116999997384846,-0.00479999989271167));
#6161=CARTESIAN_POINT('Origin',(0.,0.0116999997384946,0.));
#6162=CARTESIAN_POINT('Origin',(0.,0.0113499997351319,0.));
#6163=CARTESIAN_POINT('',(-7.9602041944578E-19,0.0109999997317891,-0.0065));
#6164=CARTESIAN_POINT('',(-7.9602041944578E-19,0.0113499997351319,-0.0065));
#6165=CARTESIAN_POINT('Origin',(0.,0.0109999997317891,0.));
#6166=CARTESIAN_POINT('Origin',(0.,0.0109999997317791,0.00455));
#6167=CARTESIAN_POINT('',(5.57214293612046E-19,0.0109999997317791,-0.00455));
#6168=CARTESIAN_POINT('Origin',(0.,0.0109999997317891,0.));
#6169=CARTESIAN_POINT('Origin',(0.,0.0112499997317791,0.));
#6170=CARTESIAN_POINT('',(4.95981953654678E-19,0.0114999997317791,-0.00405));
#6171=CARTESIAN_POINT('Origin',(0.,0.0114999997317891,0.));
#6172=CARTESIAN_POINT('',(5.26598123633362E-19,0.0112499997317791,-0.0043));
#6173=CARTESIAN_POINT('Origin',(0.,0.0117499997317791,0.));
#6174=CARTESIAN_POINT('',(-4.95981953654678E-19,0.0119999997317891,-0.00405));
#6175=CARTESIAN_POINT('',(-4.95981953654678E-19,0.0117499997317791,-0.00405));
#6176=CARTESIAN_POINT('Origin',(0.,0.0119999997317891,0.));
#6177=CARTESIAN_POINT('Origin',(0.,0.0119999997317791,0.00449999989941716));
#6178=CARTESIAN_POINT('',(5.51091047298466E-19,0.0119999997317791,-0.00449999989941718));
#6179=CARTESIAN_POINT('Origin',(0.,0.0119999997317891,0.));
#6180=CARTESIAN_POINT('Origin',(0.,0.0118499997351319,0.));
#6181=CARTESIAN_POINT('',(5.69460748875079E-19,0.0118499997351319,-0.0046499998960644));
#6182=CARTESIAN_POINT('',(0.,0.,0.));
#6183=CARTESIAN_POINT('Origin',(0.,-0.0116999997384846,0.0065));
#6184=CARTESIAN_POINT('',(-7.9602041944578E-19,-0.0116999997384946,-0.0065));
#6185=CARTESIAN_POINT('Origin',(0.,-0.0116999997384946,0.));
#6186=CARTESIAN_POINT('',(-5.87830450451699E-19,-0.0116999997384846,-0.00479999989271167));
#6187=CARTESIAN_POINT('Origin',(0.,-0.0116999997384946,0.));
#6188=CARTESIAN_POINT('Origin',(0.,-0.0113499997351319,0.));
#6189=CARTESIAN_POINT('',(-7.9602041944578E-19,-0.0109999997317891,-0.0065));
#6190=CARTESIAN_POINT('Origin',(0.,-0.0109999997317891,0.));
#6191=CARTESIAN_POINT('',(-7.9602041944578E-19,-0.0113499997351319,-0.0065));
#6192=CARTESIAN_POINT('Origin',(0.,-0.0109999997317791,0.00455));
#6193=CARTESIAN_POINT('',(-5.57214293612046E-19,-0.0109999997317791,-0.00455));
#6194=CARTESIAN_POINT('Origin',(0.,-0.0109999997317891,0.));
#6195=CARTESIAN_POINT('Origin',(0.,-0.0112499997317791,0.));
#6196=CARTESIAN_POINT('',(-4.95981953654678E-19,-0.0114999997317791,-0.00405));
#6197=CARTESIAN_POINT('Origin',(0.,-0.0114999997317891,0.));
#6198=CARTESIAN_POINT('',(-5.26598123633362E-19,-0.0112499997317791,-0.0043));
#6199=CARTESIAN_POINT('Origin',(0.,-0.0117499997317791,0.));
#6200=CARTESIAN_POINT('',(-4.95981953654678E-19,-0.0119999997317891,-0.00405));
#6201=CARTESIAN_POINT('Origin',(0.,-0.0119999997317891,0.));
#6202=CARTESIAN_POINT('',(-4.95981953654678E-19,-0.0117499997317791,-0.00405));
#6203=CARTESIAN_POINT('Origin',(0.,-0.0119999997317791,0.00449999989941716));
#6204=CARTESIAN_POINT('',(-5.51091047298466E-19,-0.0119999997317791,-0.00449999989941718));
#6205=CARTESIAN_POINT('Origin',(0.,-0.0119999997317891,0.));
#6206=CARTESIAN_POINT('Origin',(0.,-0.0118499997351319,0.));
#6207=CARTESIAN_POINT('',(-5.69460748875079E-19,-0.0118499997351319,-0.0046499998960644));
#6208=CARTESIAN_POINT('',(0.,0.,0.));
#6209=CARTESIAN_POINT('Origin',(0.,0.0109999997541308,0.00699999995096662));
#6210=CARTESIAN_POINT('',(-8.57252759403147E-19,0.0109999997541408,-0.00700000004903339));
#6211=CARTESIAN_POINT('Origin',(0.,0.0109999997541408,-4.90433850849834E-11));
#6212=CARTESIAN_POINT('',(-5.26598123633362E-19,0.0109999997541408,-0.00430000004903338));
#6213=CARTESIAN_POINT('Origin',(0.,0.0109999997541408,-4.90433850849834E-11));
#6214=CARTESIAN_POINT('Origin',(0.,0.0107499997597188,-4.90333850849834E-11));
#6215=CARTESIAN_POINT('',(-8.57252759403147E-19,0.0104999997653167,-0.00700000004903339));
#6216=CARTESIAN_POINT('',(-8.57252759403147E-19,0.0107499997597188,-0.00700000004903339));
#6217=CARTESIAN_POINT('Origin',(0.,0.0104999997653167,-4.90433850849834E-11));
#6218=CARTESIAN_POINT('Origin',(0.,0.0104999997653067,0.00429999995096661));
#6219=CARTESIAN_POINT('',(-5.26598123633362E-19,0.0104999997653167,-0.00430000004903338));
#6220=CARTESIAN_POINT('Origin',(0.,0.0104999997653167,-4.90433850849834E-11));
#6221=CARTESIAN_POINT('Origin',(0.,0.0107499997597188,-4.90333850849834E-11));
#6222=CARTESIAN_POINT('',(-5.26598123633362E-19,0.0107499997597188,-0.00430000004903338));
#6223=CARTESIAN_POINT('',(0.0218837310198402,0.0141937130870979,0.207074878461657));
#6224=CARTESIAN_POINT('',(0.0218837310198402,0.0141937130870979,0.207074878070502));
#6225=CARTESIAN_POINT('',(0.0218837310198402,0.0141937130870979,0.207074878070502));
#6226=CARTESIAN_POINT('',(0.0218837310198402,0.0141937130870979,0.207074878070502));
#6227=CARTESIAN_POINT('',(0.0218837310198402,0.0141937130870979,0.207074878461657));
#6228=CARTESIAN_POINT('',(0.0218837310198402,0.0141937130870979,0.207074878070502));
#6229=CARTESIAN_POINT('',(0.0218837310198402,0.0141937130870979,0.207074878070502));
#6230=CARTESIAN_POINT('',(0.0218837310198402,0.0141937130870979,0.207074878070502));
#6231=CARTESIAN_POINT('',(0.0218837310198402,0.0141937130870978,0.207074878461657));
#6232=CARTESIAN_POINT('',(0.0218837310198402,0.0141937130870979,0.207074878070502));
#6233=CARTESIAN_POINT('',(0.0218837310198402,0.0141937130870979,0.207074878070502));
#6234=CARTESIAN_POINT('',(0.0218837310198402,0.0141937130870979,0.207074878070502));
#6235=CARTESIAN_POINT('',(0.0218837310198401,0.0141937130870979,0.207074878461657));
#6236=CARTESIAN_POINT('',(0.0218837310198402,0.0141937130870979,0.207074878070502));
#6237=CARTESIAN_POINT('',(0.0218837310198402,0.0141937130870979,0.207074878070502));
#6238=CARTESIAN_POINT('',(0.0218837310198402,0.0141937130870979,0.207074878070502));
#6239=CARTESIAN_POINT('',(0.0218837310198402,0.0141937130870979,0.207074878461657));
#6240=CARTESIAN_POINT('',(0.0218837310198402,0.0141937130870979,0.207074878070502));
#6241=CARTESIAN_POINT('',(0.0218837310198402,0.0141937130870979,0.207074878070502));
#6242=CARTESIAN_POINT('',(0.0218837310198402,0.0141937130870979,0.207074878070502));
#6243=CARTESIAN_POINT('',(0.0218837310198402,0.0141937130870979,0.207074878461657));
#6244=CARTESIAN_POINT('',(0.0218837310198402,0.0141937130870979,0.207074878070502));
#6245=CARTESIAN_POINT('',(0.0218837310198402,0.0141937130870979,0.207074878070502));
#6246=CARTESIAN_POINT('',(0.0218837310198402,0.0141937130870979,0.207074878070502));
#6247=CARTESIAN_POINT('',(0.0218837310198402,0.014193713087098,0.207074878461657));
#6248=CARTESIAN_POINT('',(0.0218837310198402,0.0141937130870979,0.207074878070502));
#6249=CARTESIAN_POINT('',(0.0218837310198402,0.0141937130870979,0.207074878070502));
#6250=CARTESIAN_POINT('',(0.0218837310198402,0.0141937130870979,0.207074878070502));
#6251=CARTESIAN_POINT('',(0.0218837310198402,0.0141937130870978,0.207074878461657));
#6252=CARTESIAN_POINT('',(0.0218837310198402,0.0141937130870979,0.207074878070502));
#6253=CARTESIAN_POINT('',(0.0218837310198402,0.0141937130870979,0.207074878070502));
#6254=CARTESIAN_POINT('',(0.0218837310198402,0.0141937130870979,0.207074878070502));
#6255=CARTESIAN_POINT('',(0.0218837310198402,0.0141937130870978,0.207074878461657));
#6256=CARTESIAN_POINT('',(0.0218837310198402,0.0141937130870979,0.207074878070502));
#6257=CARTESIAN_POINT('',(0.0218837310198402,0.0141937130870979,0.207074878070502));
#6258=CARTESIAN_POINT('',(0.0218837310198402,0.0141937130870979,0.207074878070502));
#6259=CARTESIAN_POINT('',(0.0218837310198403,0.0141937130870979,0.207074878461657));
#6260=CARTESIAN_POINT('',(0.0218837310198402,0.0141937130870979,0.207074878070502));
#6261=CARTESIAN_POINT('',(0.0218837310198402,0.0141937130870979,0.207074878070502));
#6262=CARTESIAN_POINT('',(0.0218837310198402,0.0141937130870979,0.207074878070502));
#6263=CARTESIAN_POINT('',(0.0218837310198402,0.0141937130870978,0.207074878461657));
#6264=CARTESIAN_POINT('',(0.0218837310198402,0.0141937130870979,0.207074878070502));
#6265=CARTESIAN_POINT('',(0.0218837310198402,0.0141937130870979,0.207074878070502));
#6266=CARTESIAN_POINT('',(0.0218837310198402,0.0141937130870979,0.207074878070502));
#6267=CARTESIAN_POINT('',(0.0218837310198402,0.0141937130870979,0.207074878461657));
#6268=CARTESIAN_POINT('',(0.0218837310198402,0.0141937130870979,0.207074878070502));
#6269=CARTESIAN_POINT('',(0.0218837310198402,0.0141937130870979,0.207074878070502));
#6270=CARTESIAN_POINT('',(0.0218837310198402,0.0141937130870979,0.207074878070502));
#6271=CARTESIAN_POINT('',(0.187826861936239,0.12703574817371,0.152949877802291));
#6272=CARTESIAN_POINT('',(0.0559250074013738,0.157495785655204,0.152949877802291));
#6273=CARTESIAN_POINT('',(0.0559278442309648,0.110895785741556,0.152949877802291));
#6274=CARTESIAN_POINT('',(0.187824025106648,0.173635748087363,0.152949877802291));
#6275=CARTESIAN_POINT('',(1.24344978758018E-16,1.11022302462516E-17,-6.59364616240055E-10));
#6276=CARTESIAN_POINT('',(0.254374534550176,0.165269252629273,0.145349877802291));
#6277=CARTESIAN_POINT('',(0.245383509507527,0.0178392517997215,0.167124877802291));
#6278=CARTESIAN_POINT('',(0.245367377322084,0.282839251308684,0.190074877802291));
#6279=CARTESIAN_POINT('',(0.254374536072079,0.165244252629318,0.211849877802292));
#6280=CARTESIAN_POINT('',(0.221882748598925,0.0303378212355732,0.0817748780369842));
#6281=CARTESIAN_POINT('',(0.221868138317772,0.270337820741821,0.0802748778022911));
#6282=CARTESIAN_POINT('',(0.0218691207386847,0.254193712642384,0.0865748778022909));
#6283=CARTESIAN_POINT('',(0.187823927433681,0.175240201301577,0.152949877802291));
#6284=CARTESIAN_POINT('',(0.0559239276780895,0.175232171734558,0.152949877802291));
#6285=CARTESIAN_POINT('',(-0.0016316401699145,0.266692282029197,0.190074877802291));
#6286=CARTESIAN_POINT('',(-0.00161550798447187,0.00169228252022999,0.167124877802291));
#6287=CARTESIAN_POINT('',(0.0218837310198402,0.0141937130870979,0.0865748778022875));
#6288=CARTESIAN_POINT('',(1.55431223447522E-16,2.19824158875781E-16,-0.0569500006593647));
#6289=CARTESIAN_POINT('',(-0.0235223478209283,0.367102214166649,0.152932496939255));
#6290=CARTESIAN_POINT('',(0.199999017579088,0.016144108099431,-0.0569500006593647));
#6291=CARTESIAN_POINT('',(0.199984407297933,0.256144107654723,-0.056950000659366));
#6292=CARTESIAN_POINT('',(0.199984407297932,0.256144107654723,-6.59365859689842E-10));
#6293=CARTESIAN_POINT('',(-1.46102811559823E-5,0.239999999555286,-6.59365717581295E-10));
#6294=CARTESIAN_POINT('',(-1.46102811559112E-5,0.239999999555286,-0.0569500006593658));
#6295=CARTESIAN_POINT('',(0.223477651721388,0.367117250581006,0.175882496939255));
#6296=CARTESIAN_POINT('',(0.199999017579087,0.0161441080994309,-6.59364651767191E-10));
#6297=CARTESIAN_POINT('',(-0.0230598559958085,0.367102242321381,0.175193591953537));
#6298=CARTESIAN_POINT('',(0.223477651721388,0.367117250581006,0.152932496939255));
#6299=UNCERTAINTY_MEASURE_WITH_UNIT(LENGTH_MEASURE(1.E-5),#6349,
'DISTANCE_ACCURACY_VALUE',
'Maximum model space distance between geometric entities at asserted c
onnectivities');
#6300=UNCERTAINTY_MEASURE_WITH_UNIT(LENGTH_MEASURE(1.E-5),#6349,
'DISTANCE_ACCURACY_VALUE',
'Maximum model space distance between geometric entities at asserted c
onnectivities');
#6301=UNCERTAINTY_MEASURE_WITH_UNIT(LENGTH_MEASURE(1.E-5),#6349,
'DISTANCE_ACCURACY_VALUE',
'Maximum model space distance between geometric entities at asserted c
onnectivities');
#6302=UNCERTAINTY_MEASURE_WITH_UNIT(LENGTH_MEASURE(1.E-5),#6349,
'DISTANCE_ACCURACY_VALUE',
'Maximum model space distance between geometric entities at asserted c
onnectivities');
#6303=UNCERTAINTY_MEASURE_WITH_UNIT(LENGTH_MEASURE(1.E-5),#6349,
'DISTANCE_ACCURACY_VALUE',
'Maximum model space distance between geometric entities at asserted c
onnectivities');
#6304=UNCERTAINTY_MEASURE_WITH_UNIT(LENGTH_MEASURE(1.E-5),#6349,
'DISTANCE_ACCURACY_VALUE',
'Maximum model space distance between geometric entities at asserted c
onnectivities');
#6305=UNCERTAINTY_MEASURE_WITH_UNIT(LENGTH_MEASURE(1.E-5),#6349,
'DISTANCE_ACCURACY_VALUE',
'Maximum model space distance between geometric entities at asserted c
onnectivities');
#6306=UNCERTAINTY_MEASURE_WITH_UNIT(LENGTH_MEASURE(1.E-5),#6349,
'DISTANCE_ACCURACY_VALUE',
'Maximum model space distance between geometric entities at asserted c
onnectivities');
#6307=UNCERTAINTY_MEASURE_WITH_UNIT(LENGTH_MEASURE(1.E-5),#6349,
'DISTANCE_ACCURACY_VALUE',
'Maximum model space distance between geometric entities at asserted c
onnectivities');
#6308=UNCERTAINTY_MEASURE_WITH_UNIT(LENGTH_MEASURE(1.E-5),#6349,
'DISTANCE_ACCURACY_VALUE',
'Maximum model space distance between geometric entities at asserted c
onnectivities');
#6309=UNCERTAINTY_MEASURE_WITH_UNIT(LENGTH_MEASURE(1.E-5),#6349,
'DISTANCE_ACCURACY_VALUE',
'Maximum model space distance between geometric entities at asserted c
onnectivities');
#6310=UNCERTAINTY_MEASURE_WITH_UNIT(LENGTH_MEASURE(1.E-5),#6349,
'DISTANCE_ACCURACY_VALUE',
'Maximum model space distance between geometric entities at asserted c
onnectivities');
#6311=UNCERTAINTY_MEASURE_WITH_UNIT(LENGTH_MEASURE(1.E-5),#6349,
'DISTANCE_ACCURACY_VALUE',
'Maximum model space distance between geometric entities at asserted c
onnectivities');
#6312=UNCERTAINTY_MEASURE_WITH_UNIT(LENGTH_MEASURE(1.E-5),#6349,
'DISTANCE_ACCURACY_VALUE',
'Maximum model space distance between geometric entities at asserted c
onnectivities');
#6313=UNCERTAINTY_MEASURE_WITH_UNIT(LENGTH_MEASURE(1.E-5),#6349,
'DISTANCE_ACCURACY_VALUE',
'Maximum model space distance between geometric entities at asserted c
onnectivities');
#6314=UNCERTAINTY_MEASURE_WITH_UNIT(LENGTH_MEASURE(1.E-5),#6349,
'DISTANCE_ACCURACY_VALUE',
'Maximum model space distance between geometric entities at asserted c
onnectivities');
#6315=UNCERTAINTY_MEASURE_WITH_UNIT(LENGTH_MEASURE(1.E-5),#6349,
'DISTANCE_ACCURACY_VALUE',
'Maximum model space distance between geometric entities at asserted c
onnectivities');
#6316=UNCERTAINTY_MEASURE_WITH_UNIT(LENGTH_MEASURE(1.E-5),#6349,
'DISTANCE_ACCURACY_VALUE',
'Maximum model space distance between geometric entities at asserted c
onnectivities');
#6317=UNCERTAINTY_MEASURE_WITH_UNIT(LENGTH_MEASURE(1.E-5),#6349,
'DISTANCE_ACCURACY_VALUE',
'Maximum model space distance between geometric entities at asserted c
onnectivities');
#6318=UNCERTAINTY_MEASURE_WITH_UNIT(LENGTH_MEASURE(1.E-5),#6349,
'DISTANCE_ACCURACY_VALUE',
'Maximum model space distance between geometric entities at asserted c
onnectivities');
#6319=UNCERTAINTY_MEASURE_WITH_UNIT(LENGTH_MEASURE(1.E-5),#6349,
'DISTANCE_ACCURACY_VALUE',
'Maximum model space distance between geometric entities at asserted c
onnectivities');
#6320=UNCERTAINTY_MEASURE_WITH_UNIT(LENGTH_MEASURE(1.E-5),#6349,
'DISTANCE_ACCURACY_VALUE',
'Maximum model space distance between geometric entities at asserted c
onnectivities');
#6321=UNCERTAINTY_MEASURE_WITH_UNIT(LENGTH_MEASURE(1.E-5),#6349,
'DISTANCE_ACCURACY_VALUE',
'Maximum model space distance between geometric entities at asserted c
onnectivities');
#6322=UNCERTAINTY_MEASURE_WITH_UNIT(LENGTH_MEASURE(1.E-5),#6349,
'DISTANCE_ACCURACY_VALUE',
'Maximum model space distance between geometric entities at asserted c
onnectivities');
#6323=UNCERTAINTY_MEASURE_WITH_UNIT(LENGTH_MEASURE(1.E-5),#6349,
'DISTANCE_ACCURACY_VALUE',
'Maximum model space distance between geometric entities at asserted c
onnectivities');
#6324=(
GEOMETRIC_REPRESENTATION_CONTEXT(3)
GLOBAL_UNCERTAINTY_ASSIGNED_CONTEXT((#6299))
GLOBAL_UNIT_ASSIGNED_CONTEXT((#6349,#6350,#6351))
REPRESENTATION_CONTEXT('','3D')
);
#6325=(
GEOMETRIC_REPRESENTATION_CONTEXT(3)
GLOBAL_UNCERTAINTY_ASSIGNED_CONTEXT((#6300))
GLOBAL_UNIT_ASSIGNED_CONTEXT((#6349,#6350,#6351))
REPRESENTATION_CONTEXT('','3D')
);
#6326=(
GEOMETRIC_REPRESENTATION_CONTEXT(3)
GLOBAL_UNCERTAINTY_ASSIGNED_CONTEXT((#6301))
GLOBAL_UNIT_ASSIGNED_CONTEXT((#6349,#6350,#6351))
REPRESENTATION_CONTEXT('','3D')
);
#6327=(
GEOMETRIC_REPRESENTATION_CONTEXT(3)
GLOBAL_UNCERTAINTY_ASSIGNED_CONTEXT((#6302))
GLOBAL_UNIT_ASSIGNED_CONTEXT((#6349,#6350,#6351))
REPRESENTATION_CONTEXT('','3D')
);
#6328=(
GEOMETRIC_REPRESENTATION_CONTEXT(3)
GLOBAL_UNCERTAINTY_ASSIGNED_CONTEXT((#6303))
GLOBAL_UNIT_ASSIGNED_CONTEXT((#6349,#6350,#6351))
REPRESENTATION_CONTEXT('','3D')
);
#6329=(
GEOMETRIC_REPRESENTATION_CONTEXT(3)
GLOBAL_UNCERTAINTY_ASSIGNED_CONTEXT((#6304))
GLOBAL_UNIT_ASSIGNED_CONTEXT((#6349,#6350,#6351))
REPRESENTATION_CONTEXT('','3D')
);
#6330=(
GEOMETRIC_REPRESENTATION_CONTEXT(3)
GLOBAL_UNCERTAINTY_ASSIGNED_CONTEXT((#6305))
GLOBAL_UNIT_ASSIGNED_CONTEXT((#6349,#6350,#6351))
REPRESENTATION_CONTEXT('','3D')
);
#6331=(
GEOMETRIC_REPRESENTATION_CONTEXT(3)
GLOBAL_UNCERTAINTY_ASSIGNED_CONTEXT((#6306))
GLOBAL_UNIT_ASSIGNED_CONTEXT((#6349,#6350,#6351))
REPRESENTATION_CONTEXT('','3D')
);
#6332=(
GEOMETRIC_REPRESENTATION_CONTEXT(3)
GLOBAL_UNCERTAINTY_ASSIGNED_CONTEXT((#6307))
GLOBAL_UNIT_ASSIGNED_CONTEXT((#6349,#6350,#6351))
REPRESENTATION_CONTEXT('','3D')
);
#6333=(
GEOMETRIC_REPRESENTATION_CONTEXT(3)
GLOBAL_UNCERTAINTY_ASSIGNED_CONTEXT((#6308))
GLOBAL_UNIT_ASSIGNED_CONTEXT((#6349,#6350,#6351))
REPRESENTATION_CONTEXT('','3D')
);
#6334=(
GEOMETRIC_REPRESENTATION_CONTEXT(3)
GLOBAL_UNCERTAINTY_ASSIGNED_CONTEXT((#6309))
GLOBAL_UNIT_ASSIGNED_CONTEXT((#6349,#6350,#6351))
REPRESENTATION_CONTEXT('','3D')
);
#6335=(
GEOMETRIC_REPRESENTATION_CONTEXT(3)
GLOBAL_UNCERTAINTY_ASSIGNED_CONTEXT((#6310))
GLOBAL_UNIT_ASSIGNED_CONTEXT((#6349,#6350,#6351))
REPRESENTATION_CONTEXT('','3D')
);
#6336=(
GEOMETRIC_REPRESENTATION_CONTEXT(3)
GLOBAL_UNCERTAINTY_ASSIGNED_CONTEXT((#6311))
GLOBAL_UNIT_ASSIGNED_CONTEXT((#6349,#6350,#6351))
REPRESENTATION_CONTEXT('','3D')
);
#6337=(
GEOMETRIC_REPRESENTATION_CONTEXT(3)
GLOBAL_UNCERTAINTY_ASSIGNED_CONTEXT((#6312))
GLOBAL_UNIT_ASSIGNED_CONTEXT((#6349,#6350,#6351))
REPRESENTATION_CONTEXT('','3D')
);
#6338=(
GEOMETRIC_REPRESENTATION_CONTEXT(3)
GLOBAL_UNCERTAINTY_ASSIGNED_CONTEXT((#6313))
GLOBAL_UNIT_ASSIGNED_CONTEXT((#6349,#6350,#6351))
REPRESENTATION_CONTEXT('','3D')
);
#6339=(
GEOMETRIC_REPRESENTATION_CONTEXT(3)
GLOBAL_UNCERTAINTY_ASSIGNED_CONTEXT((#6314))
GLOBAL_UNIT_ASSIGNED_CONTEXT((#6349,#6350,#6351))
REPRESENTATION_CONTEXT('','3D')
);
#6340=(
GEOMETRIC_REPRESENTATION_CONTEXT(3)
GLOBAL_UNCERTAINTY_ASSIGNED_CONTEXT((#6315))
GLOBAL_UNIT_ASSIGNED_CONTEXT((#6349,#6350,#6351))
REPRESENTATION_CONTEXT('','3D')
);
#6341=(
GEOMETRIC_REPRESENTATION_CONTEXT(3)
GLOBAL_UNCERTAINTY_ASSIGNED_CONTEXT((#6316))
GLOBAL_UNIT_ASSIGNED_CONTEXT((#6349,#6350,#6351))
REPRESENTATION_CONTEXT('','3D')
);
#6342=(
GEOMETRIC_REPRESENTATION_CONTEXT(3)
GLOBAL_UNCERTAINTY_ASSIGNED_CONTEXT((#6317))
GLOBAL_UNIT_ASSIGNED_CONTEXT((#6349,#6350,#6351))
REPRESENTATION_CONTEXT('','3D')
);
#6343=(
GEOMETRIC_REPRESENTATION_CONTEXT(3)
GLOBAL_UNCERTAINTY_ASSIGNED_CONTEXT((#6318))
GLOBAL_UNIT_ASSIGNED_CONTEXT((#6349,#6350,#6351))
REPRESENTATION_CONTEXT('','3D')
);
#6344=(
GEOMETRIC_REPRESENTATION_CONTEXT(3)
GLOBAL_UNCERTAINTY_ASSIGNED_CONTEXT((#6319))
GLOBAL_UNIT_ASSIGNED_CONTEXT((#6349,#6350,#6351))
REPRESENTATION_CONTEXT('','3D')
);
#6345=(
GEOMETRIC_REPRESENTATION_CONTEXT(3)
GLOBAL_UNCERTAINTY_ASSIGNED_CONTEXT((#6320))
GLOBAL_UNIT_ASSIGNED_CONTEXT((#6349,#6350,#6351))
REPRESENTATION_CONTEXT('','3D')
);
#6346=(
GEOMETRIC_REPRESENTATION_CONTEXT(3)
GLOBAL_UNCERTAINTY_ASSIGNED_CONTEXT((#6321))
GLOBAL_UNIT_ASSIGNED_CONTEXT((#6349,#6350,#6351))
REPRESENTATION_CONTEXT('','3D')
);
#6347=(
GEOMETRIC_REPRESENTATION_CONTEXT(3)
GLOBAL_UNCERTAINTY_ASSIGNED_CONTEXT((#6322))
GLOBAL_UNIT_ASSIGNED_CONTEXT((#6349,#6350,#6351))
REPRESENTATION_CONTEXT('','3D')
);
#6348=(
GEOMETRIC_REPRESENTATION_CONTEXT(3)
GLOBAL_UNCERTAINTY_ASSIGNED_CONTEXT((#6323))
GLOBAL_UNIT_ASSIGNED_CONTEXT((#6349,#6350,#6351))
REPRESENTATION_CONTEXT('','3D')
);
#6349=(
LENGTH_UNIT()
NAMED_UNIT(*)
SI_UNIT($,.METRE.)
);
#6350=(
NAMED_UNIT(*)
PLANE_ANGLE_UNIT()
SI_UNIT($,.RADIAN.)
);
#6351=(
NAMED_UNIT(*)
SI_UNIT($,.STERADIAN.)
SOLID_ANGLE_UNIT()
);
#6352=SHAPE_DEFINITION_REPRESENTATION(#6376,#6476);
#6353=SHAPE_DEFINITION_REPRESENTATION(#6377,#6477);
#6354=SHAPE_DEFINITION_REPRESENTATION(#6378,#6478);
#6355=SHAPE_DEFINITION_REPRESENTATION(#6379,#6479);
#6356=SHAPE_DEFINITION_REPRESENTATION(#6380,#6480);
#6357=SHAPE_DEFINITION_REPRESENTATION(#6381,#6481);
#6358=SHAPE_DEFINITION_REPRESENTATION(#6382,#6482);
#6359=SHAPE_DEFINITION_REPRESENTATION(#6383,#6483);
#6360=SHAPE_DEFINITION_REPRESENTATION(#6384,#6484);
#6361=SHAPE_DEFINITION_REPRESENTATION(#6385,#6485);
#6362=SHAPE_DEFINITION_REPRESENTATION(#6386,#6486);
#6363=SHAPE_DEFINITION_REPRESENTATION(#6387,#6487);
#6364=SHAPE_DEFINITION_REPRESENTATION(#6388,#6488);
#6365=SHAPE_DEFINITION_REPRESENTATION(#6389,#6489);
#6366=SHAPE_DEFINITION_REPRESENTATION(#6390,#6490);
#6367=SHAPE_DEFINITION_REPRESENTATION(#6391,#6491);
#6368=SHAPE_DEFINITION_REPRESENTATION(#6392,#6492);
#6369=SHAPE_DEFINITION_REPRESENTATION(#6393,#6493);
#6370=SHAPE_DEFINITION_REPRESENTATION(#6394,#6494);
#6371=SHAPE_DEFINITION_REPRESENTATION(#6395,#6495);
#6372=SHAPE_DEFINITION_REPRESENTATION(#6396,#6496);
#6373=SHAPE_DEFINITION_REPRESENTATION(#6397,#6497);
#6374=SHAPE_DEFINITION_REPRESENTATION(#6398,#6498);
#6375=SHAPE_DEFINITION_REPRESENTATION(#6399,#6499);
#6376=PRODUCT_DEFINITION_SHAPE('',$,#6501);
#6377=PRODUCT_DEFINITION_SHAPE('',$,#6502);
#6378=PRODUCT_DEFINITION_SHAPE('',$,#6503);
#6379=PRODUCT_DEFINITION_SHAPE('',$,#6504);
#6380=PRODUCT_DEFINITION_SHAPE('',$,#6505);
#6381=PRODUCT_DEFINITION_SHAPE('',$,#6506);
#6382=PRODUCT_DEFINITION_SHAPE('',$,#6507);
#6383=PRODUCT_DEFINITION_SHAPE('',$,#6508);
#6384=PRODUCT_DEFINITION_SHAPE('',$,#6509);
#6385=PRODUCT_DEFINITION_SHAPE('',$,#6510);
#6386=PRODUCT_DEFINITION_SHAPE('',$,#6511);
#6387=PRODUCT_DEFINITION_SHAPE('',$,#6512);
#6388=PRODUCT_DEFINITION_SHAPE('',$,#6513);
#6389=PRODUCT_DEFINITION_SHAPE('',$,#6514);
#6390=PRODUCT_DEFINITION_SHAPE('',$,#6515);
#6391=PRODUCT_DEFINITION_SHAPE('',$,#6516);
#6392=PRODUCT_DEFINITION_SHAPE('',$,#6517);
#6393=PRODUCT_DEFINITION_SHAPE('',$,#6518);
#6394=PRODUCT_DEFINITION_SHAPE('',$,#6519);
#6395=PRODUCT_DEFINITION_SHAPE('',$,#6520);
#6396=PRODUCT_DEFINITION_SHAPE('',$,#6521);
#6397=PRODUCT_DEFINITION_SHAPE('',$,#6522);
#6398=PRODUCT_DEFINITION_SHAPE('',$,#6523);
#6399=PRODUCT_DEFINITION_SHAPE('',$,#6524);
#6400=PRODUCT_DEFINITION_SHAPE($,$,#239);
#6401=PRODUCT_DEFINITION_SHAPE($,$,#240);
#6402=PRODUCT_DEFINITION_SHAPE($,$,#241);
#6403=PRODUCT_DEFINITION_SHAPE($,$,#242);
#6404=PRODUCT_DEFINITION_SHAPE($,$,#243);
#6405=PRODUCT_DEFINITION_SHAPE($,$,#244);
#6406=PRODUCT_DEFINITION_SHAPE($,$,#245);
#6407=PRODUCT_DEFINITION_SHAPE($,$,#246);
#6408=PRODUCT_DEFINITION_SHAPE($,$,#247);
#6409=PRODUCT_DEFINITION_SHAPE($,$,#248);
#6410=PRODUCT_DEFINITION_SHAPE($,$,#249);
#6411=PRODUCT_DEFINITION_SHAPE($,$,#250);
#6412=PRODUCT_DEFINITION_SHAPE($,$,#251);
#6413=PRODUCT_DEFINITION_SHAPE($,$,#252);
#6414=PRODUCT_DEFINITION_SHAPE($,$,#253);
#6415=PRODUCT_DEFINITION_SHAPE($,$,#254);
#6416=PRODUCT_DEFINITION_SHAPE($,$,#255);
#6417=PRODUCT_DEFINITION_SHAPE($,$,#256);
#6418=PRODUCT_DEFINITION_SHAPE($,$,#257);
#6419=PRODUCT_DEFINITION_SHAPE($,$,#258);
#6420=PRODUCT_DEFINITION_SHAPE($,$,#259);
#6421=PRODUCT_DEFINITION_SHAPE($,$,#260);
#6422=PRODUCT_DEFINITION_SHAPE($,$,#261);
#6423=PRODUCT_DEFINITION_SHAPE($,$,#262);
#6424=PRODUCT_DEFINITION_SHAPE($,$,#263);
#6425=PRODUCT_DEFINITION_SHAPE($,$,#264);
#6426=PRODUCT_DEFINITION_SHAPE($,$,#265);
#6427=PRODUCT_DEFINITION_SHAPE($,$,#266);
#6428=PRODUCT_DEFINITION_SHAPE($,$,#267);
#6429=PRODUCT_DEFINITION_SHAPE($,$,#268);
#6430=PRODUCT_DEFINITION_SHAPE($,$,#269);
#6431=PRODUCT_DEFINITION_SHAPE($,$,#270);
#6432=PRODUCT_DEFINITION_SHAPE($,$,#271);
#6433=PRODUCT_DEFINITION_SHAPE($,$,#272);
#6434=PRODUCT_DEFINITION_SHAPE($,$,#273);
#6435=PRODUCT_DEFINITION_SHAPE($,$,#274);
#6436=PRODUCT_DEFINITION_SHAPE($,$,#275);
#6437=PRODUCT_DEFINITION_SHAPE($,$,#276);
#6438=PRODUCT_DEFINITION_SHAPE($,$,#277);
#6439=PRODUCT_DEFINITION_SHAPE($,$,#278);
#6440=PRODUCT_DEFINITION_SHAPE($,$,#279);
#6441=PRODUCT_DEFINITION_SHAPE($,$,#280);
#6442=PRODUCT_DEFINITION_SHAPE($,$,#281);
#6443=PRODUCT_DEFINITION_SHAPE($,$,#282);
#6444=PRODUCT_DEFINITION_SHAPE($,$,#283);
#6445=PRODUCT_DEFINITION_SHAPE($,$,#284);
#6446=PRODUCT_DEFINITION_SHAPE($,$,#285);
#6447=PRODUCT_DEFINITION_SHAPE($,$,#286);
#6448=PRODUCT_DEFINITION_SHAPE($,$,#287);
#6449=PRODUCT_DEFINITION_SHAPE($,$,#288);
#6450=PRODUCT_DEFINITION_SHAPE($,$,#289);
#6451=PRODUCT_DEFINITION_SHAPE($,$,#290);
#6452=PRODUCT_DEFINITION_SHAPE($,$,#291);
#6453=PRODUCT_DEFINITION_SHAPE($,$,#292);
#6454=PRODUCT_DEFINITION_SHAPE($,$,#293);
#6455=PRODUCT_DEFINITION_SHAPE($,$,#294);
#6456=PRODUCT_DEFINITION_SHAPE($,$,#295);
#6457=PRODUCT_DEFINITION_SHAPE($,$,#296);
#6458=PRODUCT_DEFINITION_SHAPE($,$,#297);
#6459=PRODUCT_DEFINITION_SHAPE($,$,#298);
#6460=PRODUCT_DEFINITION_SHAPE($,$,#299);
#6461=PRODUCT_DEFINITION_SHAPE($,$,#300);
#6462=PRODUCT_DEFINITION_SHAPE($,$,#301);
#6463=PRODUCT_DEFINITION_SHAPE($,$,#302);
#6464=PRODUCT_DEFINITION_SHAPE($,$,#303);
#6465=PRODUCT_DEFINITION_SHAPE($,$,#304);
#6466=PRODUCT_DEFINITION_SHAPE($,$,#305);
#6467=PRODUCT_DEFINITION_SHAPE($,$,#306);
#6468=PRODUCT_DEFINITION_SHAPE($,$,#307);
#6469=PRODUCT_DEFINITION_SHAPE($,$,#308);
#6470=PRODUCT_DEFINITION_SHAPE($,$,#309);
#6471=PRODUCT_DEFINITION_SHAPE($,$,#310);
#6472=PRODUCT_DEFINITION_SHAPE($,$,#311);
#6473=PRODUCT_DEFINITION_SHAPE($,$,#312);
#6474=PRODUCT_DEFINITION_SHAPE($,$,#313);
#6475=PRODUCT_DEFINITION_SHAPE($,$,#314);
#6476=SHAPE_REPRESENTATION('',(#3521,#3952,#3953,#3954,#3955,#3956,#3957,
#3958,#3959,#3960,#3961,#3962,#3963,#3964,#3965,#3966,#3967,#3968,#3969,
#3970,#3971,#3972,#3973,#3974,#3975,#3976,#3977,#3978,#3979),#6324);
#6477=SHAPE_REPRESENTATION('',(#3522),#6325);
#6478=SHAPE_REPRESENTATION('',(#3562),#6326);
#6479=SHAPE_REPRESENTATION('',(#3602),#6327);
#6480=SHAPE_REPRESENTATION('',(#3642),#6328);
#6481=SHAPE_REPRESENTATION('',(#3682,#3904,#3905,#3906,#3907),#6329);
#6482=SHAPE_REPRESENTATION('',(#3683),#6330);
#6483=SHAPE_REPRESENTATION('',(#3731),#6331);
#6484=SHAPE_REPRESENTATION('',(#3779),#6332);
#6485=SHAPE_REPRESENTATION('',(#3793,#3908,#3909,#3910,#3911),#6333);
#6486=SHAPE_REPRESENTATION('',(#3794,#3912,#3913,#3914,#3915),#6334);
#6487=SHAPE_REPRESENTATION('',(#3795,#3916,#3917,#3918,#3919),#6335);
#6488=SHAPE_REPRESENTATION('',(#3796,#3920,#3921,#3922,#3923),#6336);
#6489=SHAPE_REPRESENTATION('',(#3797,#3924,#3925,#3926,#3927),#6337);
#6490=SHAPE_REPRESENTATION('',(#3798,#3928,#3929,#3930,#3931),#6338);
#6491=SHAPE_REPRESENTATION('',(#3799,#3932,#3933,#3934,#3935),#6339);
#6492=SHAPE_REPRESENTATION('',(#3800,#3936,#3937,#3938,#3939),#6340);
#6493=SHAPE_REPRESENTATION('',(#3801,#3940,#3941,#3942,#3943),#6341);
#6494=SHAPE_REPRESENTATION('',(#3802,#3944,#3945,#3946,#3947),#6342);
#6495=SHAPE_REPRESENTATION('',(#3803,#3948,#3949,#3950,#3951),#6343);
#6496=SHAPE_REPRESENTATION('',(#3804),#6344);
#6497=SHAPE_REPRESENTATION('',(#3865),#6345);
#6498=SHAPE_REPRESENTATION('',(#3880),#6346);
#6499=SHAPE_REPRESENTATION('',(#3895),#6347);
#6500=PRODUCT_DEFINITION_CONTEXT('part definition',#6574,'design');
#6501=PRODUCT_DEFINITION('MAT-067',
'MAT-067',#6525,#6500);
#6502=PRODUCT_DEFINITION('Front Right Z Mount','Front Right Z Mount',#6526,
#6500);
#6503=PRODUCT_DEFINITION('Back Left Z Mount','Back Left Z Mount',#6527,
#6500);
#6504=PRODUCT_DEFINITION('Front Left Z Mount','Front Left Z Mount',#6528,
#6500);
#6505=PRODUCT_DEFINITION('Back Right Z Mount','Back Right Z Mount',#6529,
#6500);
#6506=PRODUCT_DEFINITION('Linear Bearing Assembly',
'Linear Bearing Assembly',#6530,#6500);
#6507=PRODUCT_DEFINITION('End Cap Right','End Cap Right',#6531,#6500);
#6508=PRODUCT_DEFINITION('End Cap Left','End Cap Left',#6532,#6500);
#6509=PRODUCT_DEFINITION('8mm Z Axis Rod','8mm Z Axis Rod',#6533,#6500);
#6510=PRODUCT_DEFINITION('Linear Bearing Assembly_1',
'Linear Bearing Assembly',#6534,#6500);
#6511=PRODUCT_DEFINITION('Linear Bearing Assembly_2',
'Linear Bearing Assembly',#6535,#6500);
#6512=PRODUCT_DEFINITION('Linear Bearing Assembly_3',
'Linear Bearing Assembly',#6536,#6500);
#6513=PRODUCT_DEFINITION('Linear Bearing Assembly_4',
'Linear Bearing Assembly',#6537,#6500);
#6514=PRODUCT_DEFINITION('Linear Bearing Assembly_5',
'Linear Bearing Assembly',#6538,#6500);
#6515=PRODUCT_DEFINITION('Linear Bearing Assembly_6',
'Linear Bearing Assembly',#6539,#6500);
#6516=PRODUCT_DEFINITION('Linear Bearing Assembly_7',
'Linear Bearing Assembly',#6540,#6500);
#6517=PRODUCT_DEFINITION('Linear Bearing Assembly_8',
'Linear Bearing Assembly',#6541,#6500);
#6518=PRODUCT_DEFINITION('Linear Bearing Assembly_9',
'Linear Bearing Assembly',#6542,#6500);
#6519=PRODUCT_DEFINITION('Linear Bearing Assembly_10',
'Linear Bearing Assembly',#6543,#6500);
#6520=PRODUCT_DEFINITION('Linear Bearing Assembly_11',
'Linear Bearing Assembly',#6544,#6500);
#6521=PRODUCT_DEFINITION('Linear Motion Ball Bushing',
'Linear Motion Ball Bushing',#6545,#6500);
#6522=PRODUCT_DEFINITION('Right Gantry Carriage Bracket',
'Right Gantry Carriage Bracket',#6546,#6500);
#6523=PRODUCT_DEFINITION('Bearing Retainer','Bearing Retainer',#6547,#6500);
#6524=PRODUCT_DEFINITION('Right Gantry Support Bracket',
'Right Gantry Support Bracket',#6548,#6500);
#6525=PRODUCT_DEFINITION_FORMATION('',$,#6576);
#6526=PRODUCT_DEFINITION_FORMATION('',$,#6577);
#6527=PRODUCT_DEFINITION_FORMATION('',$,#6578);
#6528=PRODUCT_DEFINITION_FORMATION('',$,#6579);
#6529=PRODUCT_DEFINITION_FORMATION('',$,#6580);
#6530=PRODUCT_DEFINITION_FORMATION('',$,#6581);
#6531=PRODUCT_DEFINITION_FORMATION('',$,#6582);
#6532=PRODUCT_DEFINITION_FORMATION('',$,#6583);
#6533=PRODUCT_DEFINITION_FORMATION('',$,#6584);
#6534=PRODUCT_DEFINITION_FORMATION('',$,#6585);
#6535=PRODUCT_DEFINITION_FORMATION('',$,#6586);
#6536=PRODUCT_DEFINITION_FORMATION('',$,#6587);
#6537=PRODUCT_DEFINITION_FORMATION('',$,#6588);
#6538=PRODUCT_DEFINITION_FORMATION('',$,#6589);
#6539=PRODUCT_DEFINITION_FORMATION('',$,#6590);
#6540=PRODUCT_DEFINITION_FORMATION('',$,#6591);
#6541=PRODUCT_DEFINITION_FORMATION('',$,#6592);
#6542=PRODUCT_DEFINITION_FORMATION('',$,#6593);
#6543=PRODUCT_DEFINITION_FORMATION('',$,#6594);
#6544=PRODUCT_DEFINITION_FORMATION('',$,#6595);
#6545=PRODUCT_DEFINITION_FORMATION('',$,#6596);
#6546=PRODUCT_DEFINITION_FORMATION('',$,#6597);
#6547=PRODUCT_DEFINITION_FORMATION('',$,#6598);
#6548=PRODUCT_DEFINITION_FORMATION('',$,#6599);
#6549=PRODUCT_RELATED_PRODUCT_CATEGORY('MAT-067',
'MAT-067',(#6576));
#6550=PRODUCT_RELATED_PRODUCT_CATEGORY('Front Right Z Mount',
'Front Right Z Mount',(#6577));
#6551=PRODUCT_RELATED_PRODUCT_CATEGORY('Back Left Z Mount',
'Back Left Z Mount',(#6578));
#6552=PRODUCT_RELATED_PRODUCT_CATEGORY('Front Left Z Mount',
'Front Left Z Mount',(#6579));
#6553=PRODUCT_RELATED_PRODUCT_CATEGORY('Back Right Z Mount',
'Back Right Z Mount',(#6580));
#6554=PRODUCT_RELATED_PRODUCT_CATEGORY('Linear Bearing Assembly',
'Linear Bearing Assembly',(#6581));
#6555=PRODUCT_RELATED_PRODUCT_CATEGORY('End Cap Right','End Cap Right',
(#6582));
#6556=PRODUCT_RELATED_PRODUCT_CATEGORY('End Cap Left','End Cap Left',(#6583));
#6557=PRODUCT_RELATED_PRODUCT_CATEGORY('8mm Z Axis Rod',
'8mm Z Axis Rod',(#6584));
#6558=PRODUCT_RELATED_PRODUCT_CATEGORY('Linear Bearing Assembly',
'Linear Bearing Assembly',(#6585));
#6559=PRODUCT_RELATED_PRODUCT_CATEGORY('Linear Bearing Assembly',
'Linear Bearing Assembly',(#6586));
#6560=PRODUCT_RELATED_PRODUCT_CATEGORY('Linear Bearing Assembly',
'Linear Bearing Assembly',(#6587));
#6561=PRODUCT_RELATED_PRODUCT_CATEGORY('Linear Bearing Assembly',
'Linear Bearing Assembly',(#6588));
#6562=PRODUCT_RELATED_PRODUCT_CATEGORY('Linear Bearing Assembly',
'Linear Bearing Assembly',(#6589));
#6563=PRODUCT_RELATED_PRODUCT_CATEGORY('Linear Bearing Assembly',
'Linear Bearing Assembly',(#6590));
#6564=PRODUCT_RELATED_PRODUCT_CATEGORY('Linear Bearing Assembly',
'Linear Bearing Assembly',(#6591));
#6565=PRODUCT_RELATED_PRODUCT_CATEGORY('Linear Bearing Assembly',
'Linear Bearing Assembly',(#6592));
#6566=PRODUCT_RELATED_PRODUCT_CATEGORY('Linear Bearing Assembly',
'Linear Bearing Assembly',(#6593));
#6567=PRODUCT_RELATED_PRODUCT_CATEGORY('Linear Bearing Assembly',
'Linear Bearing Assembly',(#6594));
#6568=PRODUCT_RELATED_PRODUCT_CATEGORY('Linear Bearing Assembly',
'Linear Bearing Assembly',(#6595));
#6569=PRODUCT_RELATED_PRODUCT_CATEGORY('Linear Motion Ball Bushing',
'Linear Motion Ball Bushing',(#6596));
#6570=PRODUCT_RELATED_PRODUCT_CATEGORY('Right Gantry Carriage Bracket',
'Right Gantry Carriage Bracket',(#6597));
#6571=PRODUCT_RELATED_PRODUCT_CATEGORY('Bearing Retainer',
'Bearing Retainer',(#6598));
#6572=PRODUCT_RELATED_PRODUCT_CATEGORY('Right Gantry Support Bracket',
'Right Gantry Support Bracket',(#6599));
#6573=APPLICATION_PROTOCOL_DEFINITION('international standard',
'ap242_managed_model_based_3d_engineering',2011,#6574);
#6574=APPLICATION_CONTEXT('Managed model based 3d engineering');
#6575=PRODUCT_CONTEXT('part definition',#6574,'mechanical');
#6576=PRODUCT('MAT-067',
'MAT-067',
'LEGAL AND USAGE DISCLAIMER: this Data/Model is provided \X2\201C\X0\A
S IS\X2\201D\X0\ for informational and representational only. It is a 
geometric approximation and is NOT engineered, certified, or guarantee
d for dimensional accuracy, exact tolerances, or production-level prec
ision. Vendor disclaims all implied warranties including fitness for a
 particular purpose. DO NOT USE FOR DIRECT PHYSICAL MANUFACTURING, AUT
OMATED PRODUCTION, OR SAFETY-CRITICAL SYSTEMS without independent engi
neering verification and resolution of any design discrepancies.',(#6575));
#6577=PRODUCT('Front Right Z Mount','Front Right Z Mount',
'LEGAL AND USAGE DISCLAIMER: this Data/Model is provided \X2\201C\X0\A
S IS\X2\201D\X0\ for informational and representational only. It is a 
geometric approximation and is NOT engineered, certified, or guarantee
d for dimensional accuracy, exact tolerances, or production-level prec
ision. Vendor disclaims all implied warranties including fitness for a
 particular purpose. DO NOT USE FOR DIRECT PHYSICAL MANUFACTURING, AUT
OMATED PRODUCTION, OR SAFETY-CRITICAL SYSTEMS without independent engi
neering verification and resolution of any design discrepancies.',(#6575));
#6578=PRODUCT('Back Left Z Mount','Back Left Z Mount',
'LEGAL AND USAGE DISCLAIMER: this Data/Model is provided \X2\201C\X0\A
S IS\X2\201D\X0\ for informational and representational only. It is a 
geometric approximation and is NOT engineered, certified, or guarantee
d for dimensional accuracy, exact tolerances, or production-level prec
ision. Vendor disclaims all implied warranties including fitness for a
 particular purpose. DO NOT USE FOR DIRECT PHYSICAL MANUFACTURING, AUT
OMATED PRODUCTION, OR SAFETY-CRITICAL SYSTEMS without independent engi
neering verification and resolution of any design discrepancies.',(#6575));
#6579=PRODUCT('Front Left Z Mount','Front Left Z Mount',
'LEGAL AND USAGE DISCLAIMER: this Data/Model is provided \X2\201C\X0\A
S IS\X2\201D\X0\ for informational and representational only. It is a 
geometric approximation and is NOT engineered, certified, or guarantee
d for dimensional accuracy, exact tolerances, or production-level prec
ision. Vendor disclaims all implied warranties including fitness for a
 particular purpose. DO NOT USE FOR DIRECT PHYSICAL MANUFACTURING, AUT
OMATED PRODUCTION, OR SAFETY-CRITICAL SYSTEMS without independent engi
neering verification and resolution of any design discrepancies.',(#6575));
#6580=PRODUCT('Back Right Z Mount','Back Right Z Mount',
'LEGAL AND USAGE DISCLAIMER: this Data/Model is provided \X2\201C\X0\A
S IS\X2\201D\X0\ for informational and representational only. It is a 
geometric approximation and is NOT engineered, certified, or guarantee
d for dimensional accuracy, exact tolerances, or production-level prec
ision. Vendor disclaims all implied warranties including fitness for a
 particular purpose. DO NOT USE FOR DIRECT PHYSICAL MANUFACTURING, AUT
OMATED PRODUCTION, OR SAFETY-CRITICAL SYSTEMS without independent engi
neering verification and resolution of any design discrepancies.',(#6575));
#6581=PRODUCT('Linear Bearing Assembly','Linear Bearing Assembly',
'LEGAL AND USAGE DISCLAIMER: this Data/Model is provided \X2\201C\X0\A
S IS\X2\201D\X0\ for informational and representational only. It is a 
geometric approximation and is NOT engineered, certified, or guarantee
d for dimensional accuracy, exact tolerances, or production-level prec
ision. Vendor disclaims all implied warranties including fitness for a
 particular purpose. DO NOT USE FOR DIRECT PHYSICAL MANUFACTURING, AUT
OMATED PRODUCTION, OR SAFETY-CRITICAL SYSTEMS without independent engi
neering verification and resolution of any design discrepancies.',(#6575));
#6582=PRODUCT('End Cap Right','End Cap Right',
'LEGAL AND USAGE DISCLAIMER: this Data/Model is provided \X2\201C\X0\A
S IS\X2\201D\X0\ for informational and representational only. It is a 
geometric approximation and is NOT engineered, certified, or guarantee
d for dimensional accuracy, exact tolerances, or production-level prec
ision. Vendor disclaims all implied warranties including fitness for a
 particular purpose. DO NOT USE FOR DIRECT PHYSICAL MANUFACTURING, AUT
OMATED PRODUCTION, OR SAFETY-CRITICAL SYSTEMS without independent engi
neering verification and resolution of any design discrepancies.',(#6575));
#6583=PRODUCT('End Cap Left','End Cap Left',
'LEGAL AND USAGE DISCLAIMER: this Data/Model is provided \X2\201C\X0\A
S IS\X2\201D\X0\ for informational and representational only. It is a 
geometric approximation and is NOT engineered, certified, or guarantee
d for dimensional accuracy, exact tolerances, or production-level prec
ision. Vendor disclaims all implied warranties including fitness for a
 particular purpose. DO NOT USE FOR DIRECT PHYSICAL MANUFACTURING, AUT
OMATED PRODUCTION, OR SAFETY-CRITICAL SYSTEMS without independent engi
neering verification and resolution of any design discrepancies.',(#6575));
#6584=PRODUCT('8mm Z Axis Rod','8mm Z Axis Rod',
'LEGAL AND USAGE DISCLAIMER: this Data/Model is provided \X2\201C\X0\A
S IS\X2\201D\X0\ for informational and representational only. It is a 
geometric approximation and is NOT engineered, certified, or guarantee
d for dimensional accuracy, exact tolerances, or production-level prec
ision. Vendor disclaims all implied warranties including fitness for a
 particular purpose. DO NOT USE FOR DIRECT PHYSICAL MANUFACTURING, AUT
OMATED PRODUCTION, OR SAFETY-CRITICAL SYSTEMS without independent engi
neering verification and resolution of any design discrepancies.',(#6575));
#6585=PRODUCT('Linear Bearing Assembly_1','Linear Bearing Assembly',
'LEGAL AND USAGE DISCLAIMER: this Data/Model is provided \X2\201C\X0\A
S IS\X2\201D\X0\ for informational and representational only. It is a 
geometric approximation and is NOT engineered, certified, or guarantee
d for dimensional accuracy, exact tolerances, or production-level prec
ision. Vendor disclaims all implied warranties including fitness for a
 particular purpose. DO NOT USE FOR DIRECT PHYSICAL MANUFACTURING, AUT
OMATED PRODUCTION, OR SAFETY-CRITICAL SYSTEMS without independent engi
neering verification and resolution of any design discrepancies.',(#6575));
#6586=PRODUCT('Linear Bearing Assembly_2','Linear Bearing Assembly',
'LEGAL AND USAGE DISCLAIMER: this Data/Model is provided \X2\201C\X0\A
S IS\X2\201D\X0\ for informational and representational only. It is a 
geometric approximation and is NOT engineered, certified, or guarantee
d for dimensional accuracy, exact tolerances, or production-level prec
ision. Vendor disclaims all implied warranties including fitness for a
 particular purpose. DO NOT USE FOR DIRECT PHYSICAL MANUFACTURING, AUT
OMATED PRODUCTION, OR SAFETY-CRITICAL SYSTEMS without independent engi
neering verification and resolution of any design discrepancies.',(#6575));
#6587=PRODUCT('Linear Bearing Assembly_3','Linear Bearing Assembly',
'LEGAL AND USAGE DISCLAIMER: this Data/Model is provided \X2\201C\X0\A
S IS\X2\201D\X0\ for informational and representational only. It is a 
geometric approximation and is NOT engineered, certified, or guarantee
d for dimensional accuracy, exact tolerances, or production-level prec
ision. Vendor disclaims all implied warranties including fitness for a
 particular purpose. DO NOT USE FOR DIRECT PHYSICAL MANUFACTURING, AUT
OMATED PRODUCTION, OR SAFETY-CRITICAL SYSTEMS without independent engi
neering verification and resolution of any design discrepancies.',(#6575));
#6588=PRODUCT('Linear Bearing Assembly_4','Linear Bearing Assembly',
'LEGAL AND USAGE DISCLAIMER: this Data/Model is provided \X2\201C\X0\A
S IS\X2\201D\X0\ for informational and representational only. It is a 
geometric approximation and is NOT engineered, certified, or guarantee
d for dimensional accuracy, exact tolerances, or production-level prec
ision. Vendor disclaims all implied warranties including fitness for a
 particular purpose. DO NOT USE FOR DIRECT PHYSICAL MANUFACTURING, AUT
OMATED PRODUCTION, OR SAFETY-CRITICAL SYSTEMS without independent engi
neering verification and resolution of any design discrepancies.',(#6575));
#6589=PRODUCT('Linear Bearing Assembly_5','Linear Bearing Assembly',
'LEGAL AND USAGE DISCLAIMER: this Data/Model is provided \X2\201C\X0\A
S IS\X2\201D\X0\ for informational and representational only. It is a 
geometric approximation and is NOT engineered, certified, or guarantee
d for dimensional accuracy, exact tolerances, or production-level prec
ision. Vendor disclaims all implied warranties including fitness for a
 particular purpose. DO NOT USE FOR DIRECT PHYSICAL MANUFACTURING, AUT
OMATED PRODUCTION, OR SAFETY-CRITICAL SYSTEMS without independent engi
neering verification and resolution of any design discrepancies.',(#6575));
#6590=PRODUCT('Linear Bearing Assembly_6','Linear Bearing Assembly',
'LEGAL AND USAGE DISCLAIMER: this Data/Model is provided \X2\201C\X0\A
S IS\X2\201D\X0\ for informational and representational only. It is a 
geometric approximation and is NOT engineered, certified, or guarantee
d for dimensional accuracy, exact tolerances, or production-level prec
ision. Vendor disclaims all implied warranties including fitness for a
 particular purpose. DO NOT USE FOR DIRECT PHYSICAL MANUFACTURING, AUT
OMATED PRODUCTION, OR SAFETY-CRITICAL SYSTEMS without independent engi
neering verification and resolution of any design discrepancies.',(#6575));
#6591=PRODUCT('Linear Bearing Assembly_7','Linear Bearing Assembly',
'LEGAL AND USAGE DISCLAIMER: this Data/Model is provided \X2\201C\X0\A
S IS\X2\201D\X0\ for informational and representational only. It is a 
geometric approximation and is NOT engineered, certified, or guarantee
d for dimensional accuracy, exact tolerances, or production-level prec
ision. Vendor disclaims all implied warranties including fitness for a
 particular purpose. DO NOT USE FOR DIRECT PHYSICAL MANUFACTURING, AUT
OMATED PRODUCTION, OR SAFETY-CRITICAL SYSTEMS without independent engi
neering verification and resolution of any design discrepancies.',(#6575));
#6592=PRODUCT('Linear Bearing Assembly_8','Linear Bearing Assembly',
'LEGAL AND USAGE DISCLAIMER: this Data/Model is provided \X2\201C\X0\A
S IS\X2\201D\X0\ for informational and representational only. It is a 
geometric approximation and is NOT engineered, certified, or guarantee
d for dimensional accuracy, exact tolerances, or production-level prec
ision. Vendor disclaims all implied warranties including fitness for a
 particular purpose. DO NOT USE FOR DIRECT PHYSICAL MANUFACTURING, AUT
OMATED PRODUCTION, OR SAFETY-CRITICAL SYSTEMS without independent engi
neering verification and resolution of any design discrepancies.',(#6575));
#6593=PRODUCT('Linear Bearing Assembly_9','Linear Bearing Assembly',
'LEGAL AND USAGE DISCLAIMER: this Data/Model is provided \X2\201C\X0\A
S IS\X2\201D\X0\ for informational and representational only. It is a 
geometric approximation and is NOT engineered, certified, or guarantee
d for dimensional accuracy, exact tolerances, or production-level prec
ision. Vendor disclaims all implied warranties including fitness for a
 particular purpose. DO NOT USE FOR DIRECT PHYSICAL MANUFACTURING, AUT
OMATED PRODUCTION, OR SAFETY-CRITICAL SYSTEMS without independent engi
neering verification and resolution of any design discrepancies.',(#6575));
#6594=PRODUCT('Linear Bearing Assembly_10','Linear Bearing Assembly',
'LEGAL AND USAGE DISCLAIMER: this Data/Model is provided \X2\201C\X0\A
S IS\X2\201D\X0\ for informational and representational only. It is a 
geometric approximation and is NOT engineered, certified, or guarantee
d for dimensional accuracy, exact tolerances, or production-level prec
ision. Vendor disclaims all implied warranties including fitness for a
 particular purpose. DO NOT USE FOR DIRECT PHYSICAL MANUFACTURING, AUT
OMATED PRODUCTION, OR SAFETY-CRITICAL SYSTEMS without independent engi
neering verification and resolution of any design discrepancies.',(#6575));
#6595=PRODUCT('Linear Bearing Assembly_11','Linear Bearing Assembly',
'LEGAL AND USAGE DISCLAIMER: this Data/Model is provided \X2\201C\X0\A
S IS\X2\201D\X0\ for informational and representational only. It is a 
geometric approximation and is NOT engineered, certified, or guarantee
d for dimensional accuracy, exact tolerances, or production-level prec
ision. Vendor disclaims all implied warranties including fitness for a
 particular purpose. DO NOT USE FOR DIRECT PHYSICAL MANUFACTURING, AUT
OMATED PRODUCTION, OR SAFETY-CRITICAL SYSTEMS without independent engi
neering verification and resolution of any design discrepancies.',(#6575));
#6596=PRODUCT('Linear Motion Ball Bushing','Linear Motion Ball Bushing',

'LEGAL AND USAGE DISCLAIMER: this Data/Model is provided \X2\201C\X0\A
S IS\X2\201D\X0\ for informational and representational only. It is a 
geometric approximation and is NOT engineered, certified, or guarantee
d for dimensional accuracy, exact tolerances, or production-level prec
ision. Vendor disclaims all implied warranties including fitness for a
 particular purpose. DO NOT USE FOR DIRECT PHYSICAL MANUFACTURING, AUT
OMATED PRODUCTION, OR SAFETY-CRITICAL SYSTEMS without independent engi
neering verification and resolution of any design discrepancies.',(#6575));
#6597=PRODUCT('Right Gantry Carriage Bracket',
'Right Gantry Carriage Bracket',
'LEGAL AND USAGE DISCLAIMER: this Data/Model is provided \X2\201C\X0\A
S IS\X2\201D\X0\ for informational and representational only. It is a 
geometric approximation and is NOT engineered, certified, or guarantee
d for dimensional accuracy, exact tolerances, or production-level prec
ision. Vendor disclaims all implied warranties including fitness for a
 particular purpose. DO NOT USE FOR DIRECT PHYSICAL MANUFACTURING, AUT
OMATED PRODUCTION, OR SAFETY-CRITICAL SYSTEMS without independent engi
neering verification and resolution of any design discrepancies.',(#6575));
#6598=PRODUCT('Bearing Retainer','Bearing Retainer',
'LEGAL AND USAGE DISCLAIMER: this Data/Model is provided \X2\201C\X0\A
S IS\X2\201D\X0\ for informational and representational only. It is a 
geometric approximation and is NOT engineered, certified, or guarantee
d for dimensional accuracy, exact tolerances, or production-level prec
ision. Vendor disclaims all implied warranties including fitness for a
 particular purpose. DO NOT USE FOR DIRECT PHYSICAL MANUFACTURING, AUT
OMATED PRODUCTION, OR SAFETY-CRITICAL SYSTEMS without independent engi
neering verification and resolution of any design discrepancies.',(#6575));
#6599=PRODUCT('Right Gantry Support Bracket',
'Right Gantry Support Bracket',
'LEGAL AND USAGE DISCLAIMER: this Data/Model is provided \X2\201C\X0\A
S IS\X2\201D\X0\ for informational and representational only. It is a 
geometric approximation and is NOT engineered, certified, or guarantee
d for dimensional accuracy, exact tolerances, or production-level prec
ision. Vendor disclaims all implied warranties including fitness for a
 particular purpose. DO NOT USE FOR DIRECT PHYSICAL MANUFACTURING, AUT
OMATED PRODUCTION, OR SAFETY-CRITICAL SYSTEMS without independent engi
neering verification and resolution of any design discrepancies.',(#6575));
#6600=PRESENTATION_STYLE_ASSIGNMENT((#6606));
#6601=PRESENTATION_STYLE_ASSIGNMENT((#6607));
#6602=PRESENTATION_STYLE_ASSIGNMENT((#6608));
#6603=PRESENTATION_STYLE_ASSIGNMENT((#6609));
#6604=PRESENTATION_STYLE_ASSIGNMENT((#6610));
#6605=PRESENTATION_STYLE_ASSIGNMENT((#6611));
#6606=SURFACE_STYLE_USAGE(.BOTH.,#6612);
#6607=SURFACE_STYLE_USAGE(.BOTH.,#6613);
#6608=SURFACE_STYLE_USAGE(.BOTH.,#6614);
#6609=SURFACE_STYLE_USAGE(.BOTH.,#6615);
#6610=SURFACE_STYLE_USAGE(.BOTH.,#6616);
#6611=SURFACE_STYLE_USAGE(.BOTH.,#6617);
#6612=SURFACE_SIDE_STYLE('',(#6618));
#6613=SURFACE_SIDE_STYLE('',(#6619));
#6614=SURFACE_SIDE_STYLE('',(#6620));
#6615=SURFACE_SIDE_STYLE('',(#6621));
#6616=SURFACE_SIDE_STYLE('',(#6622));
#6617=SURFACE_SIDE_STYLE('',(#6623));
#6618=SURFACE_STYLE_FILL_AREA(#6624);
#6619=SURFACE_STYLE_FILL_AREA(#6625);
#6620=SURFACE_STYLE_FILL_AREA(#6626);
#6621=SURFACE_STYLE_FILL_AREA(#6627);
#6622=SURFACE_STYLE_FILL_AREA(#6628);
#6623=SURFACE_STYLE_FILL_AREA(#6629);
#6624=FILL_AREA_STYLE('Steel - Satin',(#6630));
#6625=FILL_AREA_STYLE('Opaque(179,179,179)',(#6631));
#6626=FILL_AREA_STYLE('Opaque(246,246,243)',(#6632));
#6627=FILL_AREA_STYLE('Opaque(137,137,137)',(#6633));
#6628=FILL_AREA_STYLE('Opaque(25,25,25)',(#6634));
#6629=FILL_AREA_STYLE('Opaque(48,59,150)',(#6635));
#6630=FILL_AREA_STYLE_COLOUR('Steel - Satin',#6636);
#6631=FILL_AREA_STYLE_COLOUR('Opaque(179,179,179)',#6637);
#6632=FILL_AREA_STYLE_COLOUR('Opaque(246,246,243)',#6638);
#6633=FILL_AREA_STYLE_COLOUR('Opaque(137,137,137)',#6639);
#6634=FILL_AREA_STYLE_COLOUR('Opaque(25,25,25)',#6640);
#6635=FILL_AREA_STYLE_COLOUR('Opaque(48,59,150)',#6641);
#6636=COLOUR_RGB('Steel - Satin',0.627450980392157,0.627450980392157,0.627450980392157);
#6637=COLOUR_RGB('Opaque(179,179,179)',0.701960784313725,0.701960784313725,
0.701960784313725);
#6638=COLOUR_RGB('Opaque(246,246,243)',0.964705882352941,0.964705882352941,
0.952941176470588);
#6639=COLOUR_RGB('Opaque(137,137,137)',0.537254901960784,0.537254901960784,
0.537254901960784);
#6640=COLOUR_RGB('Opaque(25,25,25)',0.0980392156862745,0.0980392156862745,
0.0980392156862745);
#6641=COLOUR_RGB('Opaque(48,59,150)',0.188235294117647,0.231372549019608,
0.588235294117647);
ENDSEC;
END-ISO-10303-21;
